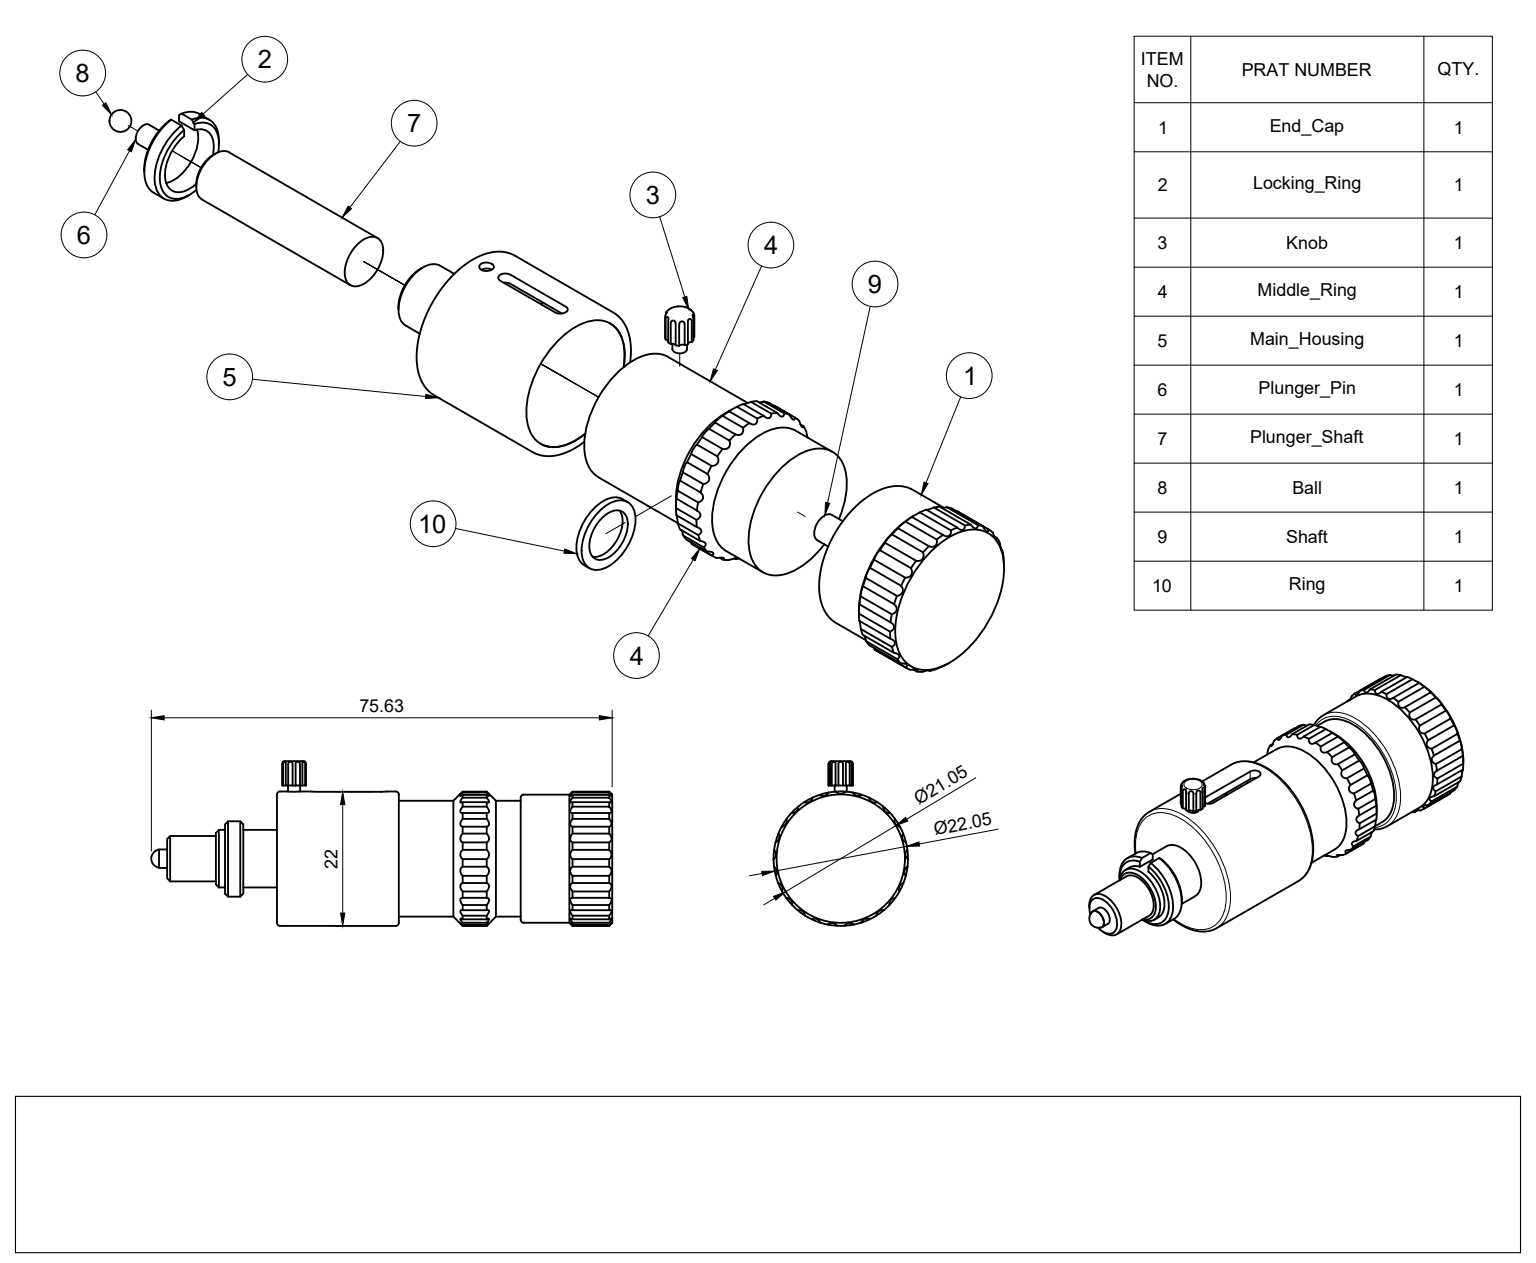
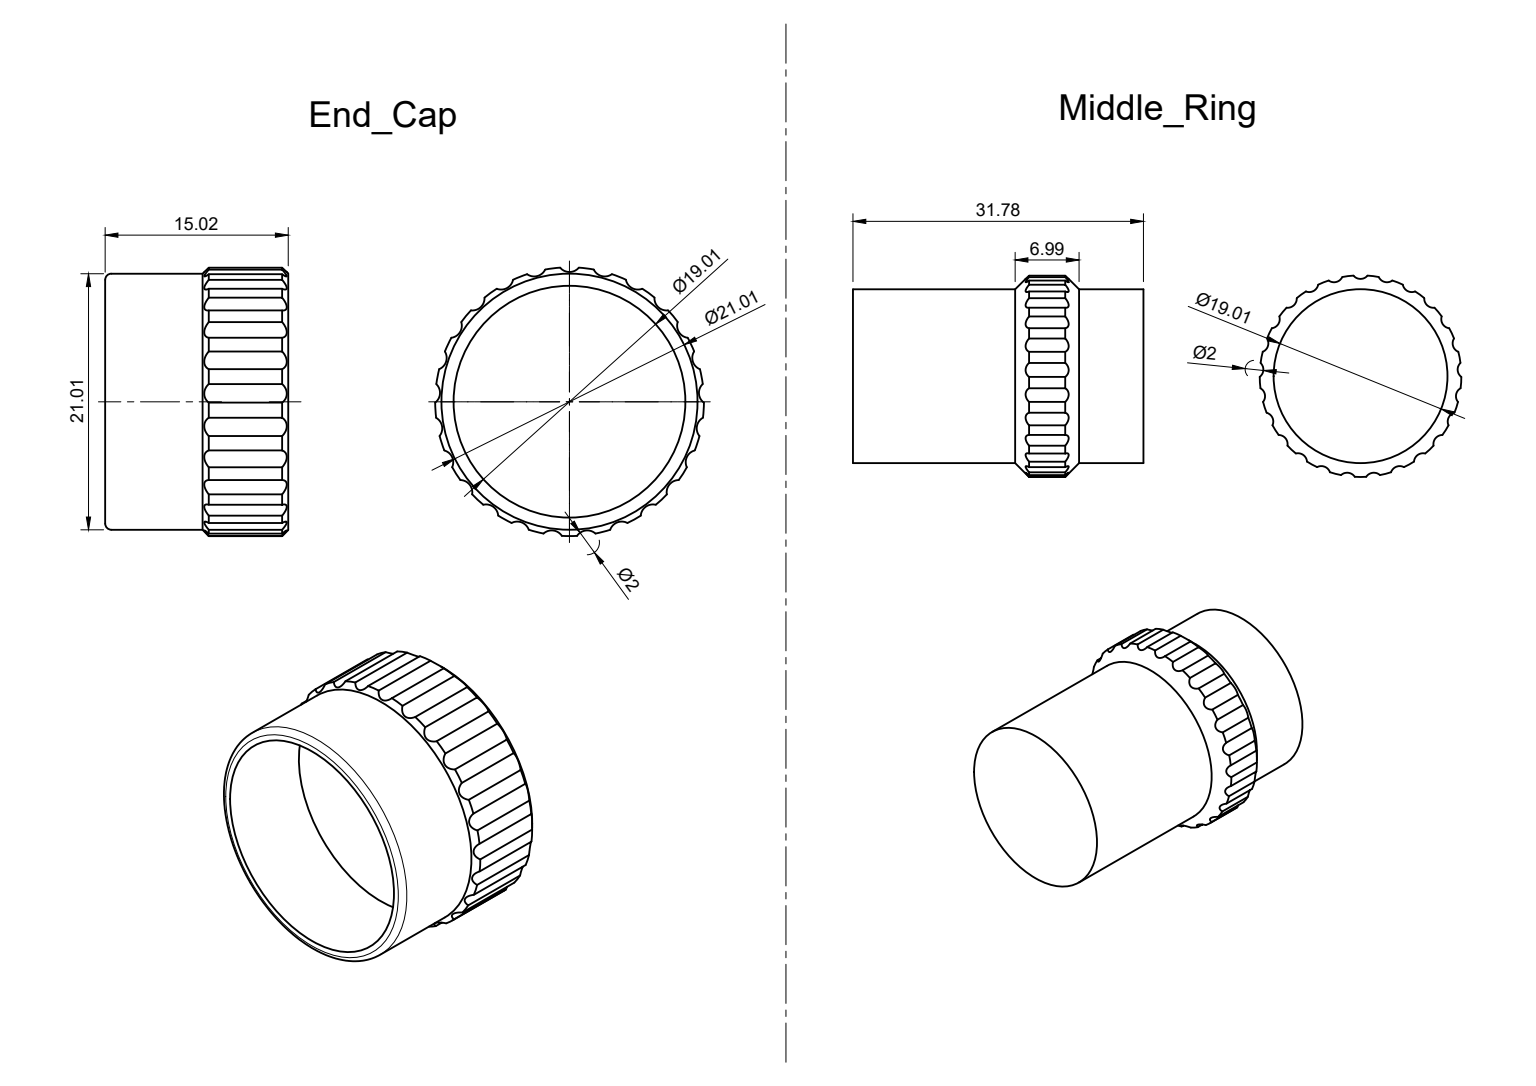
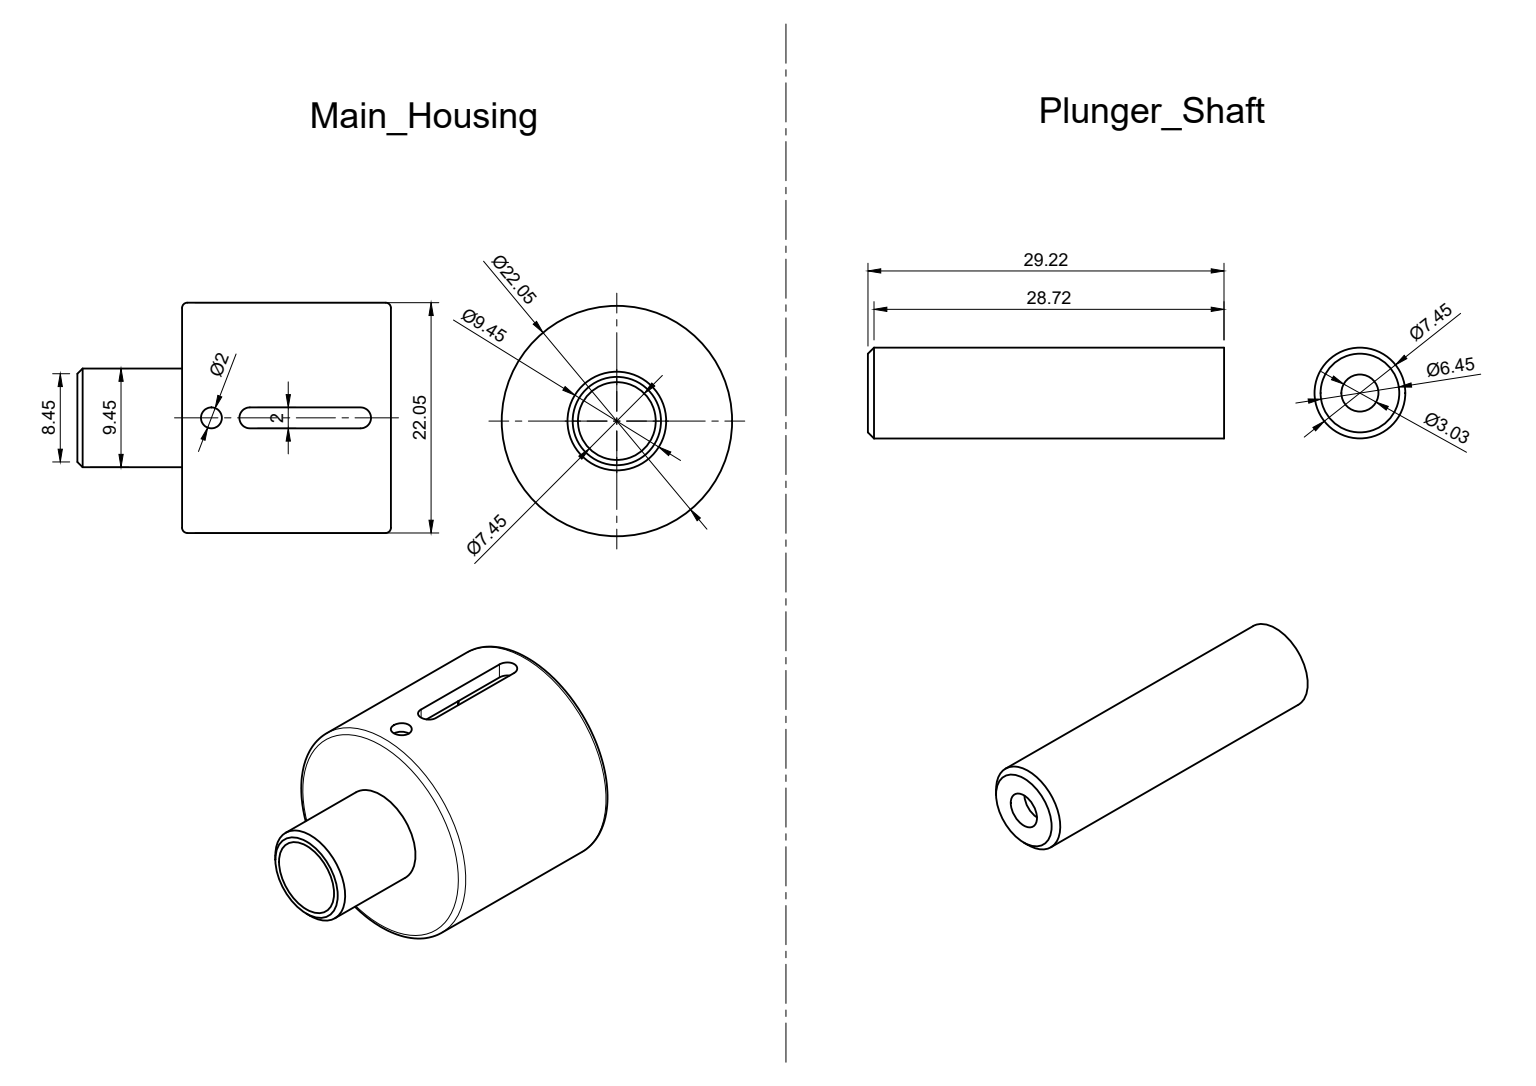
ISO-10303-21;
HEADER;
/* Generated by software containing ST-Developer
 * from STEP Tools, Inc. (www.steptools.com) 
 */

FILE_DESCRIPTION(
/* description */ (''),
/* implementation_level */ '2;1');

FILE_NAME(
/* name */ 'MAS-283',
/* time_stamp */ '2026-10-23T17:22:31+06:00',
/* author */ (''),
/* organization */ (''),
/* preprocessor_version */ 'ST-DEVELOPER v20.2',
/* originating_system */ 'Autodesk Translation Framework v15.15.0.0',
/* authorisation */ '');

FILE_SCHEMA (('AUTOMOTIVE_DESIGN { 1 0 10303 214 3 1 1 }'));
ENDSEC;

DATA;
#10=MECHANICAL_DESIGN_GEOMETRIC_PRESENTATION_REPRESENTATION('',(#77,#78,
#79,#80,#81,#82,#83,#84,#85,#86),#7315);
#11=ITEM_DEFINED_TRANSFORMATION($,$,#3336,#3714);
#12=ITEM_DEFINED_TRANSFORMATION($,$,#3452,#3715);
#13=ITEM_DEFINED_TRANSFORMATION($,$,#3467,#3716);
#14=ITEM_DEFINED_TRANSFORMATION($,$,#3527,#3717);
#15=ITEM_DEFINED_TRANSFORMATION($,$,#3638,#3718);
#16=ITEM_DEFINED_TRANSFORMATION($,$,#3673,#3719);
#17=ITEM_DEFINED_TRANSFORMATION($,$,#3684,#3720);
#18=ITEM_DEFINED_TRANSFORMATION($,$,#3696,#3721);
#19=ITEM_DEFINED_TRANSFORMATION($,$,#3699,#3722);
#20=ITEM_DEFINED_TRANSFORMATION($,$,#3705,#3723);
#21=(
REPRESENTATION_RELATIONSHIP($,$,#7353,#7352)
REPRESENTATION_RELATIONSHIP_WITH_TRANSFORMATION(#11)
SHAPE_REPRESENTATION_RELATIONSHIP()
);
#22=(
REPRESENTATION_RELATIONSHIP($,$,#7354,#7352)
REPRESENTATION_RELATIONSHIP_WITH_TRANSFORMATION(#12)
SHAPE_REPRESENTATION_RELATIONSHIP()
);
#23=(
REPRESENTATION_RELATIONSHIP($,$,#7355,#7352)
REPRESENTATION_RELATIONSHIP_WITH_TRANSFORMATION(#13)
SHAPE_REPRESENTATION_RELATIONSHIP()
);
#24=(
REPRESENTATION_RELATIONSHIP($,$,#7356,#7352)
REPRESENTATION_RELATIONSHIP_WITH_TRANSFORMATION(#14)
SHAPE_REPRESENTATION_RELATIONSHIP()
);
#25=(
REPRESENTATION_RELATIONSHIP($,$,#7357,#7352)
REPRESENTATION_RELATIONSHIP_WITH_TRANSFORMATION(#15)
SHAPE_REPRESENTATION_RELATIONSHIP()
);
#26=(
REPRESENTATION_RELATIONSHIP($,$,#7358,#7352)
REPRESENTATION_RELATIONSHIP_WITH_TRANSFORMATION(#16)
SHAPE_REPRESENTATION_RELATIONSHIP()
);
#27=(
REPRESENTATION_RELATIONSHIP($,$,#7359,#7352)
REPRESENTATION_RELATIONSHIP_WITH_TRANSFORMATION(#17)
SHAPE_REPRESENTATION_RELATIONSHIP()
);
#28=(
REPRESENTATION_RELATIONSHIP($,$,#7360,#7352)
REPRESENTATION_RELATIONSHIP_WITH_TRANSFORMATION(#18)
SHAPE_REPRESENTATION_RELATIONSHIP()
);
#29=(
REPRESENTATION_RELATIONSHIP($,$,#7361,#7352)
REPRESENTATION_RELATIONSHIP_WITH_TRANSFORMATION(#19)
SHAPE_REPRESENTATION_RELATIONSHIP()
);
#30=(
REPRESENTATION_RELATIONSHIP($,$,#7362,#7352)
REPRESENTATION_RELATIONSHIP_WITH_TRANSFORMATION(#20)
SHAPE_REPRESENTATION_RELATIONSHIP()
);
#31=CONTEXT_DEPENDENT_SHAPE_REPRESENTATION(#21,#7342);
#32=CONTEXT_DEPENDENT_SHAPE_REPRESENTATION(#22,#7343);
#33=CONTEXT_DEPENDENT_SHAPE_REPRESENTATION(#23,#7344);
#34=CONTEXT_DEPENDENT_SHAPE_REPRESENTATION(#24,#7345);
#35=CONTEXT_DEPENDENT_SHAPE_REPRESENTATION(#25,#7346);
#36=CONTEXT_DEPENDENT_SHAPE_REPRESENTATION(#26,#7347);
#37=CONTEXT_DEPENDENT_SHAPE_REPRESENTATION(#27,#7348);
#38=CONTEXT_DEPENDENT_SHAPE_REPRESENTATION(#28,#7349);
#39=CONTEXT_DEPENDENT_SHAPE_REPRESENTATION(#29,#7350);
#40=CONTEXT_DEPENDENT_SHAPE_REPRESENTATION(#30,#7351);
#41=NEXT_ASSEMBLY_USAGE_OCCURRENCE('End_Cap:1','End_Cap:1','End_Cap:1',
#7364,#7365,'End_Cap:1');
#42=NEXT_ASSEMBLY_USAGE_OCCURRENCE('Locking_Ring:1','Locking_Ring:1',
'Locking_Ring:1',#7364,#7366,'Locking_Ring:1');
#43=NEXT_ASSEMBLY_USAGE_OCCURRENCE('Knob:1','Knob:1','Knob:1',#7364,#7367,
'Knob:1');
#44=NEXT_ASSEMBLY_USAGE_OCCURRENCE('Middle_Ring:1','Middle_Ring:1',
'Middle_Ring:1',#7364,#7368,'Middle_Ring:1');
#45=NEXT_ASSEMBLY_USAGE_OCCURRENCE('Main_Housing:1','Main_Housing:1',
'Main_Housing:1',#7364,#7369,'Main_Housing:1');
#46=NEXT_ASSEMBLY_USAGE_OCCURRENCE('Plunger_Pin:1','Plunger_Pin:1',
'Plunger_Pin:1',#7364,#7370,'Plunger_Pin:1');
#47=NEXT_ASSEMBLY_USAGE_OCCURRENCE('Plunger_Shaft:1','Plunger_Shaft:1',
'Plunger_Shaft:1',#7364,#7371,'Plunger_Shaft:1');
#48=NEXT_ASSEMBLY_USAGE_OCCURRENCE('Ball:1','Ball:1','Ball:1',#7364,#7372,
'Ball:1');
#49=NEXT_ASSEMBLY_USAGE_OCCURRENCE('Shaft:1','Shaft:1','Shaft:1',#7364,
#7373,'Shaft:1');
#50=NEXT_ASSEMBLY_USAGE_OCCURRENCE('Ring:1','Ring:1','Ring:1',#7364,#7374,
'Ring:1');
#51=SPHERICAL_SURFACE('',#3674,1.5);
#52=SPHERICAL_SURFACE('',#3697,1.5);
#53=(
BOUNDED_CURVE()
B_SPLINE_CURVE(2,(#5649,#5650,#5651),.UNSPECIFIED.,.F.,.F.)
B_SPLINE_CURVE_WITH_KNOTS((3,3),(0.34166803276061,0.426429000654806),
 .UNSPECIFIED.)
CURVE()
GEOMETRIC_REPRESENTATION_ITEM()
RATIONAL_B_SPLINE_CURVE((1.00724935954325,1.0045238899297,1.))
REPRESENTATION_ITEM('')
);
#54=(
BOUNDED_CURVE()
B_SPLINE_CURVE(2,(#5655,#5656,#5657),.UNSPECIFIED.,.F.,.F.)
B_SPLINE_CURVE_WITH_KNOTS((3,3),(0.,0.0847609678918292),.UNSPECIFIED.)
CURVE()
GEOMETRIC_REPRESENTATION_ITEM()
RATIONAL_B_SPLINE_CURVE((1.,1.00452388992958,1.0072493595431))
REPRESENTATION_ITEM('')
);
#55=(
BOUNDED_CURVE()
B_SPLINE_CURVE(2,(#5669,#5670,#5671),.UNSPECIFIED.,.F.,.F.)
B_SPLINE_CURVE_WITH_KNOTS((3,3),(0.,0.0847609678918293),.UNSPECIFIED.)
CURVE()
GEOMETRIC_REPRESENTATION_ITEM()
RATIONAL_B_SPLINE_CURVE((1.,1.00452388992958,1.0072493595431))
REPRESENTATION_ITEM('')
);
#56=(
BOUNDED_CURVE()
B_SPLINE_CURVE(2,(#5678,#5679,#5680),.UNSPECIFIED.,.F.,.F.)
B_SPLINE_CURVE_WITH_KNOTS((3,3),(0.34166803276061,0.426429000654806),
 .UNSPECIFIED.)
CURVE()
GEOMETRIC_REPRESENTATION_ITEM()
RATIONAL_B_SPLINE_CURVE((1.00724935954325,1.0045238899297,1.))
REPRESENTATION_ITEM('')
);
#57=SHAPE_REPRESENTATION_RELATIONSHIP('SRR','None',#7353,#67);
#58=SHAPE_REPRESENTATION_RELATIONSHIP('SRR','None',#7354,#68);
#59=SHAPE_REPRESENTATION_RELATIONSHIP('SRR','None',#7355,#69);
#60=SHAPE_REPRESENTATION_RELATIONSHIP('SRR','None',#7356,#70);
#61=SHAPE_REPRESENTATION_RELATIONSHIP('SRR','None',#7357,#71);
#62=SHAPE_REPRESENTATION_RELATIONSHIP('SRR','None',#7358,#72);
#63=SHAPE_REPRESENTATION_RELATIONSHIP('SRR','None',#7359,#73);
#64=SHAPE_REPRESENTATION_RELATIONSHIP('SRR','None',#7360,#74);
#65=SHAPE_REPRESENTATION_RELATIONSHIP('SRR','None',#7361,#75);
#66=SHAPE_REPRESENTATION_RELATIONSHIP('SRR','None',#7362,#76);
#67=ADVANCED_BREP_SHAPE_REPRESENTATION('',(#87),#7305);
#68=ADVANCED_BREP_SHAPE_REPRESENTATION('',(#88),#7306);
#69=ADVANCED_BREP_SHAPE_REPRESENTATION('',(#89),#7307);
#70=ADVANCED_BREP_SHAPE_REPRESENTATION('',(#90),#7308);
#71=ADVANCED_BREP_SHAPE_REPRESENTATION('',(#91),#7309);
#72=ADVANCED_BREP_SHAPE_REPRESENTATION('',(#92),#7310);
#73=ADVANCED_BREP_SHAPE_REPRESENTATION('',(#93),#7311);
#74=ADVANCED_BREP_SHAPE_REPRESENTATION('',(#94),#7312);
#75=ADVANCED_BREP_SHAPE_REPRESENTATION('',(#95),#7313);
#76=ADVANCED_BREP_SHAPE_REPRESENTATION('',(#96),#7314);
#77=STYLED_ITEM('',(#7459),#87);
#78=STYLED_ITEM('',(#7438),#88);
#79=STYLED_ITEM('',(#7438),#89);
#80=STYLED_ITEM('',(#7431),#90);
#81=STYLED_ITEM('',(#7424),#91);
#82=STYLED_ITEM('',(#7445),#92);
#83=STYLED_ITEM('',(#7445),#93);
#84=STYLED_ITEM('',(#7431),#94);
#85=STYLED_ITEM('',(#7445),#95);
#86=STYLED_ITEM('',(#7431),#96);
#87=MANIFOLD_SOLID_BREP('End_Cap',#3214);
#88=MANIFOLD_SOLID_BREP('Locking_Ring',#3215);
#89=MANIFOLD_SOLID_BREP('Knob',#3216);
#90=MANIFOLD_SOLID_BREP('Middle_Ring',#3217);
#91=MANIFOLD_SOLID_BREP('Main_Housing',#3218);
#92=MANIFOLD_SOLID_BREP('Plunger_Pin',#3219);
#93=MANIFOLD_SOLID_BREP('Plunger_Shaft',#3220);
#94=MANIFOLD_SOLID_BREP('Ball',#3221);
#95=MANIFOLD_SOLID_BREP('Shaft',#3222);
#96=MANIFOLD_SOLID_BREP('Ring',#3223);
#97=CONICAL_SURFACE('',#3369,10.7746348408465,0.785398163397451);
#98=CONICAL_SURFACE('',#3445,10.765215394118,0.792062411554777);
#99=CONICAL_SURFACE('',#3453,5.97286361298787,0.785398163397449);
#100=CONICAL_SURFACE('',#3459,5.97286361298787,0.785398163397449);
#101=CONICAL_SURFACE('',#3552,10.265215394118,0.787617500807741);
#102=CONICAL_SURFACE('',#3635,10.265215394118,0.783178825987157);
#103=CONICAL_SURFACE('',#3651,4.47286361298787,0.785398163397448);
#104=CONICAL_SURFACE('',#3685,3.47286361298787,0.785398163397448);
#105=B_SPLINE_CURVE_WITH_KNOTS('',3,(#4680,#4681,#4682,#4683,#4684,#4685,
#4686,#4687,#4688,#4689,#4690,#4691,#4692,#4693),.UNSPECIFIED.,.F.,.F.,
(4,2,2,2,2,2,4),(0.0797634135970256,0.102765114722899,0.137781856198111,
0.172798597673324,0.207815339148536,0.242832080623748,0.265833781749622),
 .UNSPECIFIED.);
#106=B_SPLINE_CURVE_WITH_KNOTS('',3,(#4697,#4698,#4699,#4700,#4701,#4702,
#4703,#4704,#4705,#4706,#4707,#4708,#4709,#4710),.UNSPECIFIED.,.F.,.F.,
(4,2,2,2,2,2,4),(0.466800477660132,0.490054785503752,0.525068426419775,
0.560082067335798,0.595095708251821,0.630109349167844,0.653363657011464),
 .UNSPECIFIED.);
#107=B_SPLINE_CURVE_WITH_KNOTS('',3,(#4715,#4716,#4717,#4718,#4719,#4720,
#4721,#4722,#4723,#4724,#4725,#4726,#4727,#4728),.UNSPECIFIED.,.F.,.F.,
(4,2,2,2,2,2,4),(0.0797634135970254,0.102765114722899,0.137781856198111,
0.172798597673323,0.207815339148535,0.242832080623747,0.265833781749621),
 .UNSPECIFIED.);
#108=B_SPLINE_CURVE_WITH_KNOTS('',3,(#4732,#4733,#4734,#4735,#4736,#4737,
#4738,#4739,#4740,#4741,#4742,#4743,#4744,#4745),.UNSPECIFIED.,.F.,.F.,
(4,2,2,2,2,2,4),(0.466800477660133,0.490054785503752,0.525068426419776,
0.560082067335799,0.595095708251822,0.630109349167845,0.653363657011464),
 .UNSPECIFIED.);
#109=B_SPLINE_CURVE_WITH_KNOTS('',3,(#4750,#4751,#4752,#4753,#4754,#4755,
#4756,#4757,#4758,#4759,#4760,#4761,#4762,#4763),.UNSPECIFIED.,.F.,.F.,
(4,2,2,2,2,2,4),(0.0797634135970257,0.102765114722899,0.137781856198111,
0.172798597673324,0.207815339148536,0.242832080623748,0.265833781749623),
 .UNSPECIFIED.);
#110=B_SPLINE_CURVE_WITH_KNOTS('',3,(#4767,#4768,#4769,#4770,#4771,#4772,
#4773,#4774,#4775,#4776,#4777,#4778,#4779,#4780),.UNSPECIFIED.,.F.,.F.,
(4,2,2,2,2,2,4),(0.466800477660132,0.490054785503751,0.525068426419774,
0.560082067335798,0.595095708251821,0.630109349167844,0.653363657011463),
 .UNSPECIFIED.);
#111=B_SPLINE_CURVE_WITH_KNOTS('',3,(#4785,#4786,#4787,#4788,#4789,#4790,
#4791,#4792,#4793,#4794,#4795,#4796,#4797,#4798),.UNSPECIFIED.,.F.,.F.,
(4,2,2,2,2,2,4),(0.0797634135970255,0.102765114722899,0.137781856198111,
0.172798597673323,0.207815339148536,0.242832080623748,0.265833781749622),
 .UNSPECIFIED.);
#112=B_SPLINE_CURVE_WITH_KNOTS('',3,(#4802,#4803,#4804,#4805,#4806,#4807,
#4808,#4809,#4810,#4811,#4812,#4813,#4814,#4815),.UNSPECIFIED.,.F.,.F.,
(4,2,2,2,2,2,4),(0.466800477660132,0.490054785503752,0.525068426419775,
0.560082067335798,0.595095708251821,0.630109349167844,0.653363657011464),
 .UNSPECIFIED.);
#113=B_SPLINE_CURVE_WITH_KNOTS('',3,(#4820,#4821,#4822,#4823,#4824,#4825,
#4826,#4827,#4828,#4829,#4830,#4831,#4832,#4833),.UNSPECIFIED.,.F.,.F.,
(4,2,2,2,2,2,4),(0.0797634135970245,0.102765114722899,0.137781856198111,
0.172798597673324,0.207815339148536,0.242832080623748,0.265833781749621),
 .UNSPECIFIED.);
#114=B_SPLINE_CURVE_WITH_KNOTS('',3,(#4837,#4838,#4839,#4840,#4841,#4842,
#4843,#4844,#4845,#4846,#4847,#4848,#4849,#4850),.UNSPECIFIED.,.F.,.F.,
(4,2,2,2,2,2,4),(0.466800477660132,0.490054785503751,0.525068426419774,
0.560082067335797,0.59509570825182,0.630109349167844,0.653363657011463),
 .UNSPECIFIED.);
#115=B_SPLINE_CURVE_WITH_KNOTS('',3,(#4855,#4856,#4857,#4858,#4859,#4860,
#4861,#4862,#4863,#4864,#4865,#4866,#4867,#4868),.UNSPECIFIED.,.F.,.F.,
(4,2,2,2,2,2,4),(0.0797634135970255,0.102765114722899,0.137781856198111,
0.172798597673324,0.207815339148536,0.242832080623748,0.265833781749622),
 .UNSPECIFIED.);
#116=B_SPLINE_CURVE_WITH_KNOTS('',3,(#4872,#4873,#4874,#4875,#4876,#4877,
#4878,#4879,#4880,#4881,#4882,#4883,#4884,#4885),.UNSPECIFIED.,.F.,.F.,
(4,2,2,2,2,2,4),(0.466800477660132,0.490054785503752,0.525068426419775,
0.560082067335798,0.595095708251821,0.630109349167844,0.653363657011464),
 .UNSPECIFIED.);
#117=B_SPLINE_CURVE_WITH_KNOTS('',3,(#4890,#4891,#4892,#4893,#4894,#4895,
#4896,#4897,#4898,#4899,#4900,#4901,#4902,#4903),.UNSPECIFIED.,.F.,.F.,
(4,2,2,2,2,2,4),(0.0797634135970254,0.102765114722899,0.137781856198111,
0.172798597673323,0.207815339148536,0.242832080623748,0.265833781749621),
 .UNSPECIFIED.);
#118=B_SPLINE_CURVE_WITH_KNOTS('',3,(#4907,#4908,#4909,#4910,#4911,#4912,
#4913,#4914,#4915,#4916,#4917,#4918,#4919,#4920),.UNSPECIFIED.,.F.,.F.,
(4,2,2,2,2,2,4),(0.466800477660132,0.490054785503752,0.525068426419775,
0.560082067335798,0.595095708251821,0.630109349167844,0.653363657011464),
 .UNSPECIFIED.);
#119=B_SPLINE_CURVE_WITH_KNOTS('',3,(#4925,#4926,#4927,#4928,#4929,#4930,
#4931,#4932,#4933,#4934,#4935,#4936,#4937,#4938),.UNSPECIFIED.,.F.,.F.,
(4,2,2,2,2,2,4),(0.0797634135970265,0.1027651147229,0.137781856198112,0.172798597673324,
0.207815339148536,0.242832080623748,0.265833781749622),.UNSPECIFIED.);
#120=B_SPLINE_CURVE_WITH_KNOTS('',3,(#4942,#4943,#4944,#4945,#4946,#4947,
#4948,#4949,#4950,#4951,#4952,#4953,#4954,#4955),.UNSPECIFIED.,.F.,.F.,
(4,2,2,2,2,2,4),(0.466800477660132,0.490054785503752,0.525068426419775,
0.560082067335798,0.595095708251821,0.630109349167844,0.653363657011464),
 .UNSPECIFIED.);
#121=B_SPLINE_CURVE_WITH_KNOTS('',3,(#4960,#4961,#4962,#4963,#4964,#4965,
#4966,#4967,#4968,#4969,#4970,#4971,#4972,#4973),.UNSPECIFIED.,.F.,.F.,
(4,2,2,2,2,2,4),(0.0797634135970254,0.102765114722899,0.137781856198111,
0.172798597673323,0.207815339148535,0.242832080623747,0.265833781749621),
 .UNSPECIFIED.);
#122=B_SPLINE_CURVE_WITH_KNOTS('',3,(#4977,#4978,#4979,#4980,#4981,#4982,
#4983,#4984,#4985,#4986,#4987,#4988,#4989,#4990),.UNSPECIFIED.,.F.,.F.,
(4,2,2,2,2,2,4),(0.466800477660131,0.490054785503751,0.525068426419774,
0.560082067335798,0.59509570825182,0.630109349167843,0.653363657011463),
 .UNSPECIFIED.);
#123=B_SPLINE_CURVE_WITH_KNOTS('',3,(#4995,#4996,#4997,#4998,#4999,#5000,
#5001,#5002,#5003,#5004,#5005,#5006,#5007,#5008),.UNSPECIFIED.,.F.,.F.,
(4,2,2,2,2,2,4),(0.0797634135970272,0.102765114722899,0.137781856198112,
0.172798597673324,0.207815339148536,0.242832080623748,0.265833781749622),
 .UNSPECIFIED.);
#124=B_SPLINE_CURVE_WITH_KNOTS('',3,(#5012,#5013,#5014,#5015,#5016,#5017,
#5018,#5019,#5020,#5021,#5022,#5023,#5024,#5025),.UNSPECIFIED.,.F.,.F.,
(4,2,2,2,2,2,4),(0.466800477660132,0.490054785503752,0.525068426419775,
0.560082067335798,0.595095708251821,0.630109349167844,0.653363657011464),
 .UNSPECIFIED.);
#125=B_SPLINE_CURVE_WITH_KNOTS('',3,(#5030,#5031,#5032,#5033,#5034,#5035,
#5036,#5037,#5038,#5039,#5040,#5041,#5042,#5043),.UNSPECIFIED.,.F.,.F.,
(4,2,2,2,2,2,4),(0.0797634135970255,0.102765114722899,0.137781856198111,
0.172798597673323,0.207815339148535,0.242832080623748,0.265833781749622),
 .UNSPECIFIED.);
#126=B_SPLINE_CURVE_WITH_KNOTS('',3,(#5047,#5048,#5049,#5050,#5051,#5052,
#5053,#5054,#5055,#5056,#5057,#5058,#5059,#5060),.UNSPECIFIED.,.F.,.F.,
(4,2,2,2,2,2,4),(0.466800477660132,0.490054785503752,0.525068426419775,
0.560082067335798,0.595095708251821,0.630109349167844,0.653363657011464),
 .UNSPECIFIED.);
#127=B_SPLINE_CURVE_WITH_KNOTS('',3,(#5065,#5066,#5067,#5068,#5069,#5070,
#5071,#5072,#5073,#5074,#5075,#5076,#5077,#5078),.UNSPECIFIED.,.F.,.F.,
(4,2,2,2,2,2,4),(0.0797634135970258,0.102765114722899,0.137781856198111,
0.172798597673324,0.207815339148536,0.242832080623748,0.265833781749623),
 .UNSPECIFIED.);
#128=B_SPLINE_CURVE_WITH_KNOTS('',3,(#5082,#5083,#5084,#5085,#5086,#5087,
#5088,#5089,#5090,#5091,#5092,#5093,#5094,#5095),.UNSPECIFIED.,.F.,.F.,
(4,2,2,2,2,2,4),(0.466800477660132,0.490054785503751,0.525068426419774,
0.560082067335797,0.59509570825182,0.630109349167844,0.653363657011463),
 .UNSPECIFIED.);
#129=B_SPLINE_CURVE_WITH_KNOTS('',3,(#5100,#5101,#5102,#5103,#5104,#5105,
#5106,#5107,#5108,#5109,#5110,#5111,#5112,#5113),.UNSPECIFIED.,.F.,.F.,
(4,2,2,2,2,2,4),(0.0797634135970256,0.102765114722899,0.137781856198111,
0.172798597673324,0.207815339148536,0.242832080623748,0.265833781749621),
 .UNSPECIFIED.);
#130=B_SPLINE_CURVE_WITH_KNOTS('',3,(#5117,#5118,#5119,#5120,#5121,#5122,
#5123,#5124,#5125,#5126,#5127,#5128,#5129,#5130),.UNSPECIFIED.,.F.,.F.,
(4,2,2,2,2,2,4),(0.466800477660132,0.490054785503751,0.525068426419774,
0.560082067335797,0.595095708251821,0.630109349167844,0.653363657011463),
 .UNSPECIFIED.);
#131=B_SPLINE_CURVE_WITH_KNOTS('',3,(#5135,#5136,#5137,#5138,#5139,#5140,
#5141,#5142,#5143,#5144,#5145,#5146,#5147,#5148),.UNSPECIFIED.,.F.,.F.,
(4,2,2,2,2,2,4),(0.0797634135970255,0.102765114722899,0.137781856198111,
0.172798597673323,0.207815339148536,0.242832080623748,0.265833781749622),
 .UNSPECIFIED.);
#132=B_SPLINE_CURVE_WITH_KNOTS('',3,(#5152,#5153,#5154,#5155,#5156,#5157,
#5158,#5159,#5160,#5161,#5162,#5163,#5164,#5165),.UNSPECIFIED.,.F.,.F.,
(4,2,2,2,2,2,4),(0.466800477660132,0.490054785503751,0.525068426419775,
0.560082067335798,0.595095708251821,0.630109349167844,0.653363657011464),
 .UNSPECIFIED.);
#133=B_SPLINE_CURVE_WITH_KNOTS('',3,(#5170,#5171,#5172,#5173,#5174,#5175,
#5176,#5177,#5178,#5179,#5180,#5181,#5182,#5183),.UNSPECIFIED.,.F.,.F.,
(4,2,2,2,2,2,4),(0.0797634135970253,0.102765114722899,0.137781856198111,
0.172798597673323,0.207815339148536,0.242832080623748,0.265833781749621),
 .UNSPECIFIED.);
#134=B_SPLINE_CURVE_WITH_KNOTS('',3,(#5187,#5188,#5189,#5190,#5191,#5192,
#5193,#5194,#5195,#5196,#5197,#5198,#5199,#5200),.UNSPECIFIED.,.F.,.F.,
(4,2,2,2,2,2,4),(0.466800477660132,0.490054785503751,0.525068426419775,
0.560082067335798,0.595095708251821,0.630109349167844,0.653363657011464),
 .UNSPECIFIED.);
#135=B_SPLINE_CURVE_WITH_KNOTS('',3,(#5205,#5206,#5207,#5208,#5209,#5210,
#5211,#5212,#5213,#5214,#5215,#5216,#5217,#5218),.UNSPECIFIED.,.F.,.F.,
(4,2,2,2,2,2,4),(0.0797634135970255,0.102765114722899,0.137781856198111,
0.172798597673323,0.207815339148536,0.242832080623748,0.265833781749622),
 .UNSPECIFIED.);
#136=B_SPLINE_CURVE_WITH_KNOTS('',3,(#5222,#5223,#5224,#5225,#5226,#5227,
#5228,#5229,#5230,#5231,#5232,#5233,#5234,#5235),.UNSPECIFIED.,.F.,.F.,
(4,2,2,2,2,2,4),(0.466800477660132,0.490054785503751,0.525068426419775,
0.560082067335798,0.595095708251821,0.630109349167844,0.653363657011463),
 .UNSPECIFIED.);
#137=B_SPLINE_CURVE_WITH_KNOTS('',3,(#5240,#5241,#5242,#5243,#5244,#5245,
#5246,#5247,#5248,#5249,#5250,#5251,#5252,#5253),.UNSPECIFIED.,.F.,.F.,
(4,2,2,2,2,2,4),(0.0797634135970254,0.102765114722899,0.137781856198111,
0.172798597673323,0.207815339148535,0.242832080623747,0.265833781749621),
 .UNSPECIFIED.);
#138=B_SPLINE_CURVE_WITH_KNOTS('',3,(#5257,#5258,#5259,#5260,#5261,#5262,
#5263,#5264,#5265,#5266,#5267,#5268,#5269,#5270),.UNSPECIFIED.,.F.,.F.,
(4,2,2,2,2,2,4),(0.466800477660132,0.490054785503752,0.525068426419775,
0.560082067335798,0.595095708251821,0.630109349167844,0.653363657011464),
 .UNSPECIFIED.);
#139=B_SPLINE_CURVE_WITH_KNOTS('',3,(#5275,#5276,#5277,#5278,#5279,#5280,
#5281,#5282,#5283,#5284,#5285,#5286,#5287,#5288),.UNSPECIFIED.,.F.,.F.,
(4,2,2,2,2,2,4),(0.0797634135970276,0.102765114722899,0.137781856198111,
0.172798597673324,0.207815339148536,0.242832080623748,0.265833781749621),
 .UNSPECIFIED.);
#140=B_SPLINE_CURVE_WITH_KNOTS('',3,(#5292,#5293,#5294,#5295,#5296,#5297,
#5298,#5299,#5300,#5301,#5302,#5303,#5304,#5305),.UNSPECIFIED.,.F.,.F.,
(4,2,2,2,2,2,4),(0.466800477660133,0.490054785503752,0.525068426419776,
0.560082067335799,0.595095708251822,0.630109349167845,0.653363657011464),
 .UNSPECIFIED.);
#141=B_SPLINE_CURVE_WITH_KNOTS('',3,(#5310,#5311,#5312,#5313,#5314,#5315,
#5316,#5317,#5318,#5319,#5320,#5321,#5322,#5323),.UNSPECIFIED.,.F.,.F.,
(4,2,2,2,2,2,4),(0.0797634135970256,0.102765114722899,0.137781856198112,
0.172798597673324,0.207815339148536,0.242832080623748,0.265833781749622),
 .UNSPECIFIED.);
#142=B_SPLINE_CURVE_WITH_KNOTS('',3,(#5327,#5328,#5329,#5330,#5331,#5332,
#5333,#5334,#5335,#5336,#5337,#5338,#5339,#5340),.UNSPECIFIED.,.F.,.F.,
(4,2,2,2,2,2,4),(0.466800477660132,0.490054785503752,0.525068426419775,
0.560082067335798,0.595095708251822,0.630109349167845,0.653363657011465),
 .UNSPECIFIED.);
#143=B_SPLINE_CURVE_WITH_KNOTS('',3,(#5345,#5346,#5347,#5348,#5349,#5350,
#5351,#5352,#5353,#5354,#5355,#5356,#5357,#5358),.UNSPECIFIED.,.F.,.F.,
(4,2,2,2,2,2,4),(0.0797634135970255,0.102765114722899,0.137781856198111,
0.172798597673323,0.207815339148536,0.242832080623748,0.265833781749621),
 .UNSPECIFIED.);
#144=B_SPLINE_CURVE_WITH_KNOTS('',3,(#5362,#5363,#5364,#5365,#5366,#5367,
#5368,#5369,#5370,#5371,#5372,#5373,#5374,#5375),.UNSPECIFIED.,.F.,.F.,
(4,2,2,2,2,2,4),(0.466800477660133,0.490054785503752,0.525068426419775,
0.560082067335798,0.595095708251821,0.630109349167844,0.653363657011464),
 .UNSPECIFIED.);
#145=B_SPLINE_CURVE_WITH_KNOTS('',3,(#5380,#5381,#5382,#5383,#5384,#5385,
#5386,#5387,#5388,#5389,#5390,#5391,#5392,#5393),.UNSPECIFIED.,.F.,.F.,
(4,2,2,2,2,2,4),(0.0797634135970255,0.102765114722899,0.137781856198111,
0.172798597673323,0.207815339148536,0.242832080623748,0.265833781749621),
 .UNSPECIFIED.);
#146=B_SPLINE_CURVE_WITH_KNOTS('',3,(#5397,#5398,#5399,#5400,#5401,#5402,
#5403,#5404,#5405,#5406,#5407,#5408,#5409,#5410),.UNSPECIFIED.,.F.,.F.,
(4,2,2,2,2,2,4),(0.466800477660132,0.490054785503752,0.525068426419775,
0.560082067335798,0.595095708251821,0.630109349167844,0.653363657011464),
 .UNSPECIFIED.);
#147=B_SPLINE_CURVE_WITH_KNOTS('',3,(#5415,#5416,#5417,#5418,#5419,#5420,
#5421,#5422,#5423,#5424,#5425,#5426,#5427,#5428),.UNSPECIFIED.,.F.,.F.,
(4,2,2,2,2,2,4),(0.0797634135970255,0.102765114722899,0.137781856198111,
0.172798597673324,0.207815339148536,0.242832080623748,0.265833781749623),
 .UNSPECIFIED.);
#148=B_SPLINE_CURVE_WITH_KNOTS('',3,(#5432,#5433,#5434,#5435,#5436,#5437,
#5438,#5439,#5440,#5441,#5442,#5443,#5444,#5445),.UNSPECIFIED.,.F.,.F.,
(4,2,2,2,2,2,4),(0.466800477660132,0.490054785503752,0.525068426419775,
0.560082067335798,0.595095708251821,0.630109349167844,0.653363657011463),
 .UNSPECIFIED.);
#149=B_SPLINE_CURVE_WITH_KNOTS('',3,(#5450,#5451,#5452,#5453,#5454,#5455,
#5456,#5457,#5458,#5459,#5460,#5461,#5462,#5463),.UNSPECIFIED.,.F.,.F.,
(4,2,2,2,2,2,4),(0.0797634135970256,0.102765114722899,0.137781856198111,
0.172798597673323,0.207815339148536,0.242832080623748,0.265833781749621),
 .UNSPECIFIED.);
#150=B_SPLINE_CURVE_WITH_KNOTS('',3,(#5467,#5468,#5469,#5470,#5471,#5472,
#5473,#5474,#5475,#5476,#5477,#5478,#5479,#5480),.UNSPECIFIED.,.F.,.F.,
(4,2,2,2,2,2,4),(0.466800477660132,0.490054785503752,0.525068426419775,
0.560082067335798,0.595095708251821,0.630109349167844,0.653363657011463),
 .UNSPECIFIED.);
#151=B_SPLINE_CURVE_WITH_KNOTS('',3,(#5485,#5486,#5487,#5488,#5489,#5490,
#5491,#5492,#5493,#5494,#5495,#5496,#5497,#5498),.UNSPECIFIED.,.F.,.F.,
(4,2,2,2,2,2,4),(0.0797634135970257,0.102765114722899,0.137781856198111,
0.172798597673324,0.207815339148536,0.242832080623748,0.265833781749622),
 .UNSPECIFIED.);
#152=B_SPLINE_CURVE_WITH_KNOTS('',3,(#5502,#5503,#5504,#5505,#5506,#5507,
#5508,#5509,#5510,#5511,#5512,#5513,#5514,#5515),.UNSPECIFIED.,.F.,.F.,
(4,2,2,2,2,2,4),(0.466800477660132,0.490054785503752,0.525068426419775,
0.560082067335798,0.595095708251821,0.630109349167844,0.653363657011463),
 .UNSPECIFIED.);
#153=B_SPLINE_CURVE_WITH_KNOTS('',3,(#5523,#5524,#5525,#5526,#5527,#5528,
#5529,#5530),.UNSPECIFIED.,.F.,.F.,(4,2,2,4),(0.560082067335798,0.595095708251821,
0.630109349167844,0.653363657011463),.UNSPECIFIED.);
#154=B_SPLINE_CURVE_WITH_KNOTS('',3,(#5557,#5558,#5559,#5560,#5561,#5562,
#5563,#5564),.UNSPECIFIED.,.F.,.F.,(4,2,2,4),(0.466800477660132,0.490054785503752,
0.525068426419775,0.560082067335798),.UNSPECIFIED.);
#155=B_SPLINE_CURVE_WITH_KNOTS('',3,(#5619,#5620,#5621,#5622,#5623,#5624,
#5625,#5626),.UNSPECIFIED.,.F.,.F.,(4,2,2,4),(0.0797634135970255,0.102765114722899,
0.137781856198111,0.172798597673323),.UNSPECIFIED.);
#156=B_SPLINE_CURVE_WITH_KNOTS('',3,(#5627,#5628,#5629,#5630,#5631,#5632,
#5633,#5634),.UNSPECIFIED.,.F.,.F.,(4,2,2,4),(0.172798597673323,0.207815339148535,
0.242832080623748,0.265833781749621),.UNSPECIFIED.);
#157=B_SPLINE_CURVE_WITH_KNOTS('',3,(#5698,#5699,#5700,#5701,#5702,#5703,
#5704,#5705,#5706,#5707,#5708,#5709,#5710,#5711,#5712,#5713,#5714,#5715,
#5716,#5717,#5718,#5719),.UNSPECIFIED.,.F.,.F.,(4,2,2,2,2,2,2,2,2,2,4),
(-0.134540802780941,-0.124694593380528,-0.114887429972743,-0.100865411229465,
-0.0874132288816555,-0.0739776319181918,-0.0597069979702496,-0.0456321639023999,
-0.0321262367963484,-0.0169842646851755,-7.43769472487735E-6),
 .UNSPECIFIED.);
#158=B_SPLINE_CURVE_WITH_KNOTS('',3,(#5728,#5729,#5730,#5731,#5732,#5733,
#5734,#5735,#5736,#5737,#5738,#5739,#5740,#5741,#5742,#5743,#5744,#5745,
#5746,#5747,#5748,#5749),.UNSPECIFIED.,.F.,.F.,(4,2,2,2,2,2,2,2,2,2,4),
(-0.134546412264088,-0.12503895955274,-0.115553020431079,-0.101555833168035,
-0.0880617151829101,-0.0742479340082139,-0.0594501685168066,-0.0457182707143297,
-0.0321286187319872,-0.0169925187729982,-7.43769474437564E-6),
 .UNSPECIFIED.);
#159=B_SPLINE_CURVE_WITH_KNOTS('',3,(#5758,#5759,#5760,#5761,#5762,#5763,
#5764,#5765,#5766,#5767,#5768,#5769,#5770,#5771,#5772,#5773,#5774,#5775,
#5776,#5777,#5778,#5779),.UNSPECIFIED.,.F.,.F.,(4,2,2,2,2,2,2,2,2,2,4),
(-0.134546412264079,-0.125038959552735,-0.115553020431074,-0.101555833168028,
-0.0880617151829049,-0.074247934008211,-0.0594501685168069,-0.0457182707143326,
-0.0321286187319901,-0.0169925187729991,-7.43769474460115E-6),
 .UNSPECIFIED.);
#160=B_SPLINE_CURVE_WITH_KNOTS('',3,(#5788,#5789,#5790,#5791,#5792,#5793,
#5794,#5795,#5796,#5797,#5798,#5799,#5800,#5801,#5802,#5803,#5804,#5805,
#5806,#5807,#5808,#5809),.UNSPECIFIED.,.F.,.F.,(4,2,2,2,2,2,2,2,2,2,4),
(-0.134540616537392,-0.124646722470156,-0.114789241819855,-0.100787758586552,
-0.0873465389988059,-0.0739206374616,-0.0596515865040428,-0.0456502398664556,
-0.0321268160753299,-0.0169860369506264,-7.43769472906497E-6),
 .UNSPECIFIED.);
#161=B_SPLINE_CURVE_WITH_KNOTS('',3,(#5818,#5819,#5820,#5821,#5822,#5823,
#5824,#5825,#5826,#5827,#5828,#5829,#5830,#5831,#5832,#5833,#5834,#5835,
#5836,#5837,#5838,#5839,#5840,#5841,#5842,#5843),.UNSPECIFIED.,.F.,.F.,
(4,2,2,2,2,2,2,2,2,2,2,2,4),(-0.134481588819224,-0.12541821251768,-0.116248820382152,
-0.10297112990022,-0.0890270299810203,-0.0783509942952859,-0.0707062224441527,
-0.0638270554385495,-0.0561931432260482,-0.0455507450931791,-0.031889734739909,
-0.0168775831944051,-7.43769447408144E-6),.UNSPECIFIED.);
#162=B_SPLINE_CURVE_WITH_KNOTS('',3,(#5852,#5853,#5854,#5855,#5856,#5857,
#5858,#5859,#5860,#5861,#5862,#5863,#5864,#5865,#5866,#5867,#5868,#5869,
#5870,#5871,#5872,#5873),.UNSPECIFIED.,.F.,.F.,(4,2,2,2,2,2,2,2,2,2,4),
(-0.134540616537393,-0.124646722470158,-0.114789241819856,-0.100787758586554,
-0.087346538998809,-0.0739206374616026,-0.0596515865040475,-0.0456502398664592,
-0.0321268160753317,-0.0169860369506279,-7.43769472906497E-6),
 .UNSPECIFIED.);
#163=B_SPLINE_CURVE_WITH_KNOTS('',3,(#5882,#5883,#5884,#5885,#5886,#5887,
#5888,#5889,#5890,#5891,#5892,#5893,#5894,#5895,#5896,#5897,#5898,#5899,
#5900,#5901,#5902,#5903),.UNSPECIFIED.,.F.,.F.,(4,2,2,2,2,2,2,2,2,2,4),
(-0.134546412264079,-0.125038959552731,-0.115553020431069,-0.101555833168023,
-0.0880617151828988,-0.0742479340082045,-0.0594501685167969,-0.0457182707143222,
-0.0321286187319822,-0.0169925187729959,-7.43769474437564E-6),
 .UNSPECIFIED.);
#164=B_SPLINE_CURVE_WITH_KNOTS('',3,(#5912,#5913,#5914,#5915,#5916,#5917,
#5918,#5919,#5920,#5921,#5922,#5923,#5924,#5925,#5926,#5927,#5928,#5929,
#5930,#5931,#5932,#5933),.UNSPECIFIED.,.F.,.F.,(4,2,2,2,2,2,2,2,2,2,4),
(-0.134546412264076,-0.125038959552731,-0.11555302043107,-0.101555833168024,
-0.0880617151829001,-0.0742479340082053,-0.0594501685167959,-0.0457182707143225,
-0.0321286187319831,-0.0169925187729947,-7.43769474415359E-6),
 .UNSPECIFIED.);
#165=B_SPLINE_CURVE_WITH_KNOTS('',3,(#5942,#5943,#5944,#5945,#5946,#5947,
#5948,#5949,#5950,#5951,#5952,#5953,#5954,#5955,#5956,#5957,#5958,#5959,
#5960,#5961,#5962,#5963),.UNSPECIFIED.,.F.,.F.,(4,2,2,2,2,2,2,2,2,2,4),
(-0.134540802780906,-0.124694593380492,-0.114887429972709,-0.100865411229438,
-0.0874132288816369,-0.0739776319181792,-0.0597069979702393,-0.0456321639023924,
-0.0321262367963445,-0.0169842646851756,-7.43769472488082E-6),
 .UNSPECIFIED.);
#166=B_SPLINE_CURVE_WITH_KNOTS('',3,(#6008,#6009,#6010,#6011,#6012,#6013,
#6014,#6015,#6016,#6017,#6018,#6019),.UNSPECIFIED.,.F.,.F.,(4,2,2,2,2,4),
(-0.0672537780264869,-0.0571863690452376,-0.0459002523768814,-0.0321135744364736,
-0.0170527660266752,0.),.UNSPECIFIED.);
#167=B_SPLINE_CURVE_WITH_KNOTS('',3,(#6022,#6023,#6024,#6025,#6026,#6027,
#6028,#6029,#6030,#6031,#6032,#6033,#6034,#6035,#6036,#6037),
 .UNSPECIFIED.,.F.,.F.,(4,2,2,2,2,2,2,4),(-0.134507884019342,-0.12584488585901,
-0.117135322530839,-0.103482612739793,-0.0895114384281185,-0.0780993566612536,
-0.0676309733624946,-0.0672537780264869),.UNSPECIFIED.);
#168=B_SPLINE_CURVE_WITH_KNOTS('',3,(#6051,#6052,#6053,#6054,#6055,#6056,
#6057,#6058,#6059,#6060,#6061,#6062,#6063,#6064),.UNSPECIFIED.,.F.,.F.,
(4,2,2,2,2,2,4),(0.0804140797636754,0.103753655307869,0.138766322922265,
0.173778990536662,0.208791658151058,0.243804325765454,0.267143901309648),
 .UNSPECIFIED.);
#169=B_SPLINE_CURVE_WITH_KNOTS('',3,(#6068,#6069,#6070,#6071,#6072,#6073,
#6074,#6075,#6076,#6077,#6078,#6079,#6080,#6081),.UNSPECIFIED.,.F.,.F.,
(4,2,2,2,2,2,4),(0.466102891398403,0.489272506433,0.524287150622646,0.559301794812291,
0.594316439001936,0.629331083191581,0.652500698226179),.UNSPECIFIED.);
#170=B_SPLINE_CURVE_WITH_KNOTS('',3,(#6086,#6087,#6088,#6089,#6090,#6091,
#6092,#6093,#6094,#6095,#6096,#6097,#6098,#6099),.UNSPECIFIED.,.F.,.F.,
(4,2,2,2,2,2,4),(0.0804140797636753,0.103753655307869,0.138766322922265,
0.173778990536662,0.208791658151058,0.243804325765454,0.267143901309648),
 .UNSPECIFIED.);
#171=B_SPLINE_CURVE_WITH_KNOTS('',3,(#6103,#6104,#6105,#6106,#6107,#6108,
#6109,#6110,#6111,#6112,#6113,#6114,#6115,#6116),.UNSPECIFIED.,.F.,.F.,
(4,2,2,2,2,2,4),(0.466102891398403,0.489272506433,0.524287150622645,0.55930179481229,
0.594316439001936,0.629331083191581,0.652500698226178),.UNSPECIFIED.);
#172=B_SPLINE_CURVE_WITH_KNOTS('',3,(#6121,#6122,#6123,#6124,#6125,#6126,
#6127,#6128,#6129,#6130,#6131,#6132,#6133,#6134),.UNSPECIFIED.,.F.,.F.,
(4,2,2,2,2,2,4),(0.0804140797636755,0.103753655307869,0.138766322922265,
0.173778990536661,0.208791658151058,0.243804325765454,0.267143901309647),
 .UNSPECIFIED.);
#173=B_SPLINE_CURVE_WITH_KNOTS('',3,(#6138,#6139,#6140,#6141,#6142,#6143,
#6144,#6145,#6146,#6147,#6148,#6149,#6150,#6151),.UNSPECIFIED.,.F.,.F.,
(4,2,2,2,2,2,4),(0.466102891398403,0.489272506433,0.524287150622646,0.559301794812291,
0.594316439001936,0.629331083191582,0.652500698226179),.UNSPECIFIED.);
#174=B_SPLINE_CURVE_WITH_KNOTS('',3,(#6156,#6157,#6158,#6159,#6160,#6161,
#6162,#6163,#6164,#6165,#6166,#6167,#6168,#6169),.UNSPECIFIED.,.F.,.F.,
(4,2,2,2,2,2,4),(0.0804140797636754,0.103753655307869,0.138766322922265,
0.173778990536662,0.208791658151058,0.243804325765454,0.267143901309648),
 .UNSPECIFIED.);
#175=B_SPLINE_CURVE_WITH_KNOTS('',3,(#6173,#6174,#6175,#6176,#6177,#6178,
#6179,#6180,#6181,#6182,#6183,#6184,#6185,#6186),.UNSPECIFIED.,.F.,.F.,
(4,2,2,2,2,2,4),(0.466102891398402,0.489272506433,0.524287150622646,0.559301794812291,
0.594316439001936,0.629331083191581,0.652500698226179),.UNSPECIFIED.);
#176=B_SPLINE_CURVE_WITH_KNOTS('',3,(#6191,#6192,#6193,#6194,#6195,#6196,
#6197,#6198,#6199,#6200,#6201,#6202,#6203,#6204),.UNSPECIFIED.,.F.,.F.,
(4,2,2,2,2,2,4),(0.0804140797636755,0.103753655307869,0.138766322922265,
0.173778990536661,0.208791658151058,0.243804325765454,0.267143901309648),
 .UNSPECIFIED.);
#177=B_SPLINE_CURVE_WITH_KNOTS('',3,(#6208,#6209,#6210,#6211,#6212,#6213,
#6214,#6215,#6216,#6217,#6218,#6219,#6220,#6221),.UNSPECIFIED.,.F.,.F.,
(4,2,2,2,2,2,4),(0.466102891398402,0.489272506433,0.524287150622645,0.55930179481229,
0.594316439001935,0.629331083191581,0.652500698226178),.UNSPECIFIED.);
#178=B_SPLINE_CURVE_WITH_KNOTS('',3,(#6226,#6227,#6228,#6229,#6230,#6231,
#6232,#6233,#6234,#6235,#6236,#6237,#6238,#6239),.UNSPECIFIED.,.F.,.F.,
(4,2,2,2,2,2,4),(0.0804140797636754,0.103753655307869,0.138766322922265,
0.173778990536662,0.208791658151058,0.243804325765454,0.267143901309648),
 .UNSPECIFIED.);
#179=B_SPLINE_CURVE_WITH_KNOTS('',3,(#6243,#6244,#6245,#6246,#6247,#6248,
#6249,#6250,#6251,#6252,#6253,#6254,#6255,#6256),.UNSPECIFIED.,.F.,.F.,
(4,2,2,2,2,2,4),(0.466102891398402,0.489272506433,0.524287150622645,0.559301794812291,
0.594316439001936,0.629331083191581,0.652500698226179),.UNSPECIFIED.);
#180=B_SPLINE_CURVE_WITH_KNOTS('',3,(#6261,#6262,#6263,#6264,#6265,#6266,
#6267,#6268,#6269,#6270,#6271,#6272,#6273,#6274),.UNSPECIFIED.,.F.,.F.,
(4,2,2,2,2,2,4),(0.0804140797636753,0.103753655307869,0.138766322922265,
0.173778990536662,0.208791658151058,0.243804325765455,0.267143901309648),
 .UNSPECIFIED.);
#181=B_SPLINE_CURVE_WITH_KNOTS('',3,(#6278,#6279,#6280,#6281,#6282,#6283,
#6284,#6285,#6286,#6287,#6288,#6289,#6290,#6291),.UNSPECIFIED.,.F.,.F.,
(4,2,2,2,2,2,4),(0.466102891398403,0.489272506433,0.524287150622645,0.559301794812291,
0.594316439001936,0.629331083191581,0.652500698226179),.UNSPECIFIED.);
#182=B_SPLINE_CURVE_WITH_KNOTS('',3,(#6296,#6297,#6298,#6299,#6300,#6301,
#6302,#6303,#6304,#6305,#6306,#6307,#6308,#6309),.UNSPECIFIED.,.F.,.F.,
(4,2,2,2,2,2,4),(0.0804140797636755,0.103753655307869,0.138766322922265,
0.173778990536662,0.208791658151058,0.243804325765455,0.267143901309648),
 .UNSPECIFIED.);
#183=B_SPLINE_CURVE_WITH_KNOTS('',3,(#6313,#6314,#6315,#6316,#6317,#6318,
#6319,#6320,#6321,#6322,#6323,#6324,#6325,#6326),.UNSPECIFIED.,.F.,.F.,
(4,2,2,2,2,2,4),(0.466102891398403,0.489272506433,0.524287150622645,0.55930179481229,
0.594316439001936,0.629331083191581,0.652500698226179),.UNSPECIFIED.);
#184=B_SPLINE_CURVE_WITH_KNOTS('',3,(#6331,#6332,#6333,#6334,#6335,#6336,
#6337,#6338,#6339,#6340,#6341,#6342,#6343,#6344),.UNSPECIFIED.,.F.,.F.,
(4,2,2,2,2,2,4),(0.0804140797636754,0.103753655307869,0.138766322922265,
0.173778990536661,0.208791658151058,0.243804325765454,0.267143901309648),
 .UNSPECIFIED.);
#185=B_SPLINE_CURVE_WITH_KNOTS('',3,(#6348,#6349,#6350,#6351,#6352,#6353,
#6354,#6355,#6356,#6357,#6358,#6359,#6360,#6361),.UNSPECIFIED.,.F.,.F.,
(4,2,2,2,2,2,4),(0.466102891398402,0.489272506433,0.524287150622645,0.55930179481229,
0.594316439001936,0.629331083191581,0.652500698226179),.UNSPECIFIED.);
#186=B_SPLINE_CURVE_WITH_KNOTS('',3,(#6366,#6367,#6368,#6369,#6370,#6371,
#6372,#6373,#6374,#6375,#6376,#6377,#6378,#6379),.UNSPECIFIED.,.F.,.F.,
(4,2,2,2,2,2,4),(0.0804140797636754,0.103753655307869,0.138766322922265,
0.173778990536662,0.208791658151058,0.243804325765454,0.267143901309648),
 .UNSPECIFIED.);
#187=B_SPLINE_CURVE_WITH_KNOTS('',3,(#6383,#6384,#6385,#6386,#6387,#6388,
#6389,#6390,#6391,#6392,#6393,#6394,#6395,#6396),.UNSPECIFIED.,.F.,.F.,
(4,2,2,2,2,2,4),(0.466102891398402,0.489272506433,0.524287150622645,0.55930179481229,
0.594316439001935,0.62933108319158,0.652500698226178),.UNSPECIFIED.);
#188=B_SPLINE_CURVE_WITH_KNOTS('',3,(#6401,#6402,#6403,#6404,#6405,#6406,
#6407,#6408,#6409,#6410,#6411,#6412,#6413,#6414),.UNSPECIFIED.,.F.,.F.,
(4,2,2,2,2,2,4),(0.0804140797636753,0.103753655307869,0.138766322922265,
0.173778990536661,0.208791658151058,0.243804325765454,0.267143901309648),
 .UNSPECIFIED.);
#189=B_SPLINE_CURVE_WITH_KNOTS('',3,(#6418,#6419,#6420,#6421,#6422,#6423,
#6424,#6425,#6426,#6427,#6428,#6429,#6430,#6431),.UNSPECIFIED.,.F.,.F.,
(4,2,2,2,2,2,4),(0.466102891398402,0.489272506432999,0.524287150622645,
0.55930179481229,0.594316439001935,0.62933108319158,0.652500698226178),
 .UNSPECIFIED.);
#190=B_SPLINE_CURVE_WITH_KNOTS('',3,(#6436,#6437,#6438,#6439,#6440,#6441,
#6442,#6443,#6444,#6445,#6446,#6447,#6448,#6449),.UNSPECIFIED.,.F.,.F.,
(4,2,2,2,2,2,4),(0.0804140797636754,0.103753655307869,0.138766322922265,
0.173778990536661,0.208791658151058,0.243804325765454,0.267143901309648),
 .UNSPECIFIED.);
#191=B_SPLINE_CURVE_WITH_KNOTS('',3,(#6453,#6454,#6455,#6456,#6457,#6458,
#6459,#6460,#6461,#6462,#6463,#6464,#6465,#6466),.UNSPECIFIED.,.F.,.F.,
(4,2,2,2,2,2,4),(0.466102891398402,0.489272506433,0.524287150622645,0.55930179481229,
0.594316439001935,0.629331083191581,0.652500698226178),.UNSPECIFIED.);
#192=B_SPLINE_CURVE_WITH_KNOTS('',3,(#6471,#6472,#6473,#6474,#6475,#6476,
#6477,#6478,#6479,#6480,#6481,#6482,#6483,#6484),.UNSPECIFIED.,.F.,.F.,
(4,2,2,2,2,2,4),(0.0804140797636754,0.103753655307869,0.138766322922265,
0.173778990536662,0.208791658151058,0.243804325765454,0.267143901309648),
 .UNSPECIFIED.);
#193=B_SPLINE_CURVE_WITH_KNOTS('',3,(#6488,#6489,#6490,#6491,#6492,#6493,
#6494,#6495,#6496,#6497,#6498,#6499,#6500,#6501),.UNSPECIFIED.,.F.,.F.,
(4,2,2,2,2,2,4),(0.466102891398403,0.489272506433,0.524287150622646,0.559301794812291,
0.594316439001936,0.629331083191581,0.652500698226179),.UNSPECIFIED.);
#194=B_SPLINE_CURVE_WITH_KNOTS('',3,(#6506,#6507,#6508,#6509,#6510,#6511,
#6512,#6513,#6514,#6515,#6516,#6517,#6518,#6519),.UNSPECIFIED.,.F.,.F.,
(4,2,2,2,2,2,4),(0.0804140797636752,0.103753655307869,0.138766322922265,
0.173778990536661,0.208791658151058,0.243804325765454,0.267143901309648),
 .UNSPECIFIED.);
#195=B_SPLINE_CURVE_WITH_KNOTS('',3,(#6523,#6524,#6525,#6526,#6527,#6528,
#6529,#6530,#6531,#6532,#6533,#6534,#6535,#6536),.UNSPECIFIED.,.F.,.F.,
(4,2,2,2,2,2,4),(0.466102891398402,0.489272506432999,0.524287150622644,
0.559301794812289,0.594316439001935,0.62933108319158,0.652500698226178),
 .UNSPECIFIED.);
#196=B_SPLINE_CURVE_WITH_KNOTS('',3,(#6541,#6542,#6543,#6544,#6545,#6546,
#6547,#6548,#6549,#6550,#6551,#6552,#6553,#6554),.UNSPECIFIED.,.F.,.F.,
(4,2,2,2,2,2,4),(0.0804140797636753,0.103753655307869,0.138766322922265,
0.173778990536662,0.208791658151058,0.243804325765455,0.267143901309648),
 .UNSPECIFIED.);
#197=B_SPLINE_CURVE_WITH_KNOTS('',3,(#6558,#6559,#6560,#6561,#6562,#6563,
#6564,#6565,#6566,#6567,#6568,#6569,#6570,#6571),.UNSPECIFIED.,.F.,.F.,
(4,2,2,2,2,2,4),(0.466102891398402,0.489272506432999,0.524287150622644,
0.55930179481229,0.594316439001935,0.62933108319158,0.652500698226178),
 .UNSPECIFIED.);
#198=B_SPLINE_CURVE_WITH_KNOTS('',3,(#6576,#6577,#6578,#6579,#6580,#6581,
#6582,#6583,#6584,#6585,#6586,#6587,#6588,#6589),.UNSPECIFIED.,.F.,.F.,
(4,2,2,2,2,2,4),(0.0804140797636755,0.103753655307869,0.138766322922265,
0.173778990536661,0.208791658151058,0.243804325765454,0.267143901309648),
 .UNSPECIFIED.);
#199=B_SPLINE_CURVE_WITH_KNOTS('',3,(#6593,#6594,#6595,#6596,#6597,#6598,
#6599,#6600,#6601,#6602,#6603,#6604,#6605,#6606),.UNSPECIFIED.,.F.,.F.,
(4,2,2,2,2,2,4),(0.466102891398403,0.489272506433,0.524287150622646,0.559301794812291,
0.594316439001936,0.629331083191581,0.652500698226179),.UNSPECIFIED.);
#200=B_SPLINE_CURVE_WITH_KNOTS('',3,(#6611,#6612,#6613,#6614,#6615,#6616,
#6617,#6618,#6619,#6620,#6621,#6622,#6623,#6624),.UNSPECIFIED.,.F.,.F.,
(4,2,2,2,2,2,4),(0.0804140797636754,0.103753655307869,0.138766322922265,
0.173778990536662,0.208791658151058,0.243804325765454,0.267143901309648),
 .UNSPECIFIED.);
#201=B_SPLINE_CURVE_WITH_KNOTS('',3,(#6628,#6629,#6630,#6631,#6632,#6633,
#6634,#6635,#6636,#6637,#6638,#6639,#6640,#6641),.UNSPECIFIED.,.F.,.F.,
(4,2,2,2,2,2,4),(0.466102891398403,0.489272506433,0.524287150622646,0.559301794812291,
0.594316439001936,0.629331083191581,0.652500698226179),.UNSPECIFIED.);
#202=B_SPLINE_CURVE_WITH_KNOTS('',3,(#6646,#6647,#6648,#6649,#6650,#6651,
#6652,#6653,#6654,#6655,#6656,#6657,#6658,#6659),.UNSPECIFIED.,.F.,.F.,
(4,2,2,2,2,2,4),(0.0804140797636755,0.103753655307869,0.138766322922265,
0.173778990536662,0.208791658151058,0.243804325765454,0.267143901309648),
 .UNSPECIFIED.);
#203=B_SPLINE_CURVE_WITH_KNOTS('',3,(#6663,#6664,#6665,#6666,#6667,#6668,
#6669,#6670,#6671,#6672,#6673,#6674,#6675,#6676),.UNSPECIFIED.,.F.,.F.,
(4,2,2,2,2,2,4),(0.466102891398403,0.489272506433,0.524287150622645,0.55930179481229,
0.594316439001935,0.62933108319158,0.652500698226178),.UNSPECIFIED.);
#204=B_SPLINE_CURVE_WITH_KNOTS('',3,(#6681,#6682,#6683,#6684,#6685,#6686,
#6687,#6688,#6689,#6690,#6691,#6692,#6693,#6694),.UNSPECIFIED.,.F.,.F.,
(4,2,2,2,2,2,4),(0.0804140797636754,0.103753655307869,0.138766322922265,
0.173778990536662,0.208791658151058,0.243804325765455,0.267143901309648),
 .UNSPECIFIED.);
#205=B_SPLINE_CURVE_WITH_KNOTS('',3,(#6698,#6699,#6700,#6701,#6702,#6703,
#6704,#6705,#6706,#6707,#6708,#6709,#6710,#6711),.UNSPECIFIED.,.F.,.F.,
(4,2,2,2,2,2,4),(0.466102891398403,0.489272506433001,0.524287150622646,
0.559301794812291,0.594316439001936,0.629331083191582,0.65250069822618),
 .UNSPECIFIED.);
#206=B_SPLINE_CURVE_WITH_KNOTS('',3,(#6716,#6717,#6718,#6719,#6720,#6721,
#6722,#6723,#6724,#6725,#6726,#6727,#6728,#6729),.UNSPECIFIED.,.F.,.F.,
(4,2,2,2,2,2,4),(0.0804140797636755,0.103753655307869,0.138766322922265,
0.173778990536661,0.208791658151058,0.243804325765455,0.267143901309648),
 .UNSPECIFIED.);
#207=B_SPLINE_CURVE_WITH_KNOTS('',3,(#6733,#6734,#6735,#6736,#6737,#6738,
#6739,#6740,#6741,#6742,#6743,#6744,#6745,#6746),.UNSPECIFIED.,.F.,.F.,
(4,2,2,2,2,2,4),(0.466102891398403,0.489272506433,0.524287150622645,0.559301794812291,
0.594316439001936,0.629331083191581,0.652500698226178),.UNSPECIFIED.);
#208=B_SPLINE_CURVE_WITH_KNOTS('',3,(#6751,#6752,#6753,#6754,#6755,#6756,
#6757,#6758,#6759,#6760,#6761,#6762,#6763,#6764),.UNSPECIFIED.,.F.,.F.,
(4,2,2,2,2,2,4),(0.0804140797636753,0.103753655307869,0.138766322922265,
0.173778990536662,0.208791658151058,0.243804325765455,0.267143901309648),
 .UNSPECIFIED.);
#209=B_SPLINE_CURVE_WITH_KNOTS('',3,(#6768,#6769,#6770,#6771,#6772,#6773,
#6774,#6775,#6776,#6777,#6778,#6779,#6780,#6781),.UNSPECIFIED.,.F.,.F.,
(4,2,2,2,2,2,4),(0.466102891398403,0.489272506433,0.524287150622646,0.559301794812291,
0.594316439001936,0.629331083191581,0.652500698226179),.UNSPECIFIED.);
#210=B_SPLINE_CURVE_WITH_KNOTS('',3,(#6786,#6787,#6788,#6789,#6790,#6791,
#6792,#6793,#6794,#6795,#6796,#6797,#6798,#6799),.UNSPECIFIED.,.F.,.F.,
(4,2,2,2,2,2,4),(0.0804140797636753,0.103753655307869,0.138766322922265,
0.173778990536662,0.208791658151058,0.243804325765455,0.267143901309648),
 .UNSPECIFIED.);
#211=B_SPLINE_CURVE_WITH_KNOTS('',3,(#6803,#6804,#6805,#6806,#6807,#6808,
#6809,#6810,#6811,#6812,#6813,#6814,#6815,#6816),.UNSPECIFIED.,.F.,.F.,
(4,2,2,2,2,2,4),(0.466102891398403,0.489272506433,0.524287150622646,0.559301794812291,
0.594316439001936,0.629331083191581,0.652500698226179),.UNSPECIFIED.);
#212=B_SPLINE_CURVE_WITH_KNOTS('',3,(#6821,#6822,#6823,#6824,#6825,#6826,
#6827,#6828,#6829,#6830,#6831,#6832,#6833,#6834),.UNSPECIFIED.,.F.,.F.,
(4,2,2,2,2,2,4),(0.0804140797636755,0.103753655307869,0.138766322922265,
0.173778990536661,0.208791658151058,0.243804325765454,0.267143901309648),
 .UNSPECIFIED.);
#213=B_SPLINE_CURVE_WITH_KNOTS('',3,(#6838,#6839,#6840,#6841,#6842,#6843,
#6844,#6845,#6846,#6847,#6848,#6849,#6850,#6851),.UNSPECIFIED.,.F.,.F.,
(4,2,2,2,2,2,4),(0.466102891398403,0.489272506433,0.524287150622646,0.559301794812291,
0.594316439001936,0.629331083191581,0.652500698226179),.UNSPECIFIED.);
#214=B_SPLINE_CURVE_WITH_KNOTS('',3,(#6856,#6857,#6858,#6859,#6860,#6861,
#6862,#6863,#6864,#6865,#6866,#6867,#6868,#6869),.UNSPECIFIED.,.F.,.F.,
(4,2,2,2,2,2,4),(0.0804140797636756,0.103753655307869,0.138766322922265,
0.173778990536662,0.208791658151058,0.243804325765454,0.267143901309648),
 .UNSPECIFIED.);
#215=B_SPLINE_CURVE_WITH_KNOTS('',3,(#6873,#6874,#6875,#6876,#6877,#6878,
#6879,#6880,#6881,#6882,#6883,#6884,#6885,#6886),.UNSPECIFIED.,.F.,.F.,
(4,2,2,2,2,2,4),(0.466102891398403,0.489272506433,0.524287150622645,0.55930179481229,
0.594316439001936,0.629331083191581,0.652500698226178),.UNSPECIFIED.);
#216=B_SPLINE_CURVE_WITH_KNOTS('',3,(#6894,#6895,#6896,#6897,#6898,#6899,
#6900,#6901),.UNSPECIFIED.,.F.,.F.,(4,2,2,4),(0.559301794812291,0.594316439001936,
0.629331083191581,0.652500698226179),.UNSPECIFIED.);
#217=B_SPLINE_CURVE_WITH_KNOTS('',3,(#6928,#6929,#6930,#6931,#6932,#6933,
#6934,#6935),.UNSPECIFIED.,.F.,.F.,(4,2,2,4),(0.466102891398403,0.489272506433001,
0.524287150622646,0.559301794812291),.UNSPECIFIED.);
#218=B_SPLINE_CURVE_WITH_KNOTS('',3,(#6990,#6991,#6992,#6993,#6994,#6995,
#6996,#6997),.UNSPECIFIED.,.F.,.F.,(4,2,2,4),(0.0804140797636754,0.103753655307869,
0.138766322922265,0.173778990536661),.UNSPECIFIED.);
#219=B_SPLINE_CURVE_WITH_KNOTS('',3,(#6998,#6999,#7000,#7001,#7002,#7003,
#7004,#7005),.UNSPECIFIED.,.F.,.F.,(4,2,2,4),(0.173778990536661,0.208791658151058,
0.243804325765454,0.267143901309647),.UNSPECIFIED.);
#220=B_SPLINE_CURVE_WITH_KNOTS('',3,(#7037,#7038,#7039,#7040,#7041,#7042,
#7043,#7044,#7045,#7046,#7047,#7048,#7049,#7050,#7051,#7052,#7053,#7054),
 .UNSPECIFIED.,.F.,.F.,(4,2,2,2,2,2,2,2,4),(0.,0.0376986977587122,0.0753973955174244,
0.11309593596243,0.150794476407437,0.188493016852443,0.226191557297449,
0.263890255056161,0.301588952814873),.UNSPECIFIED.);
#221=B_SPLINE_CURVE_WITH_KNOTS('',3,(#7057,#7058,#7059,#7060,#7061,#7062,
#7063,#7064,#7065,#7066,#7067,#7068,#7069,#7070,#7071,#7072,#7073,#7074),
 .UNSPECIFIED.,.F.,.F.,(4,2,2,2,2,2,2,2,4),(-0.301588952814873,-0.263890255056161,
-0.226191557297449,-0.188493016852443,-0.150794476407437,-0.113095935962431,
-0.0753973955174246,-0.0376986977587124,0.),.UNSPECIFIED.);
#222=B_SPLINE_CURVE_WITH_KNOTS('',3,(#7085,#7086,#7087,#7088,#7089,#7090,
#7091,#7092,#7093,#7094),.UNSPECIFIED.,.F.,.F.,(4,2,2,2,4),(-0.150763619405615,
-0.113072757903898,-0.0753818964021818,-0.037690948201091,0.),
 .UNSPECIFIED.);
#223=B_SPLINE_CURVE_WITH_KNOTS('',3,(#7095,#7096,#7097,#7098,#7099,#7100,
#7101,#7102,#7103,#7104),.UNSPECIFIED.,.F.,.F.,(4,2,2,2,4),(-0.30152723881123,
-0.263836290610139,-0.226145342409048,-0.188454480907332,-0.150763619405615),
 .UNSPECIFIED.);
#224=B_SPLINE_CURVE_WITH_KNOTS('',3,(#7108,#7109,#7110,#7111,#7112,#7113,
#7114,#7115,#7116,#7117),.UNSPECIFIED.,.F.,.F.,(4,2,2,2,4),(0.,0.037690948201091,
0.075381896402182,0.113072757903899,0.150763619405615),.UNSPECIFIED.);
#225=B_SPLINE_CURVE_WITH_KNOTS('',3,(#7119,#7120,#7121,#7122,#7123,#7124,
#7125,#7126,#7127,#7128),.UNSPECIFIED.,.F.,.F.,(4,2,2,2,4),(0.452290858216846,
0.489981719718562,0.527672581220279,0.56536352942137,0.603054477622461),
 .UNSPECIFIED.);
#226=B_SPLINE_CURVE_WITH_KNOTS('',3,(#7132,#7133,#7134,#7135,#7136,#7137,
#7138,#7139,#7140,#7141,#7142,#7143,#7144,#7145,#7146,#7147,#7148,#7149),
 .UNSPECIFIED.,.F.,.F.,(4,2,2,2,2,2,2,2,4),(0.150763619405615,0.188454480907332,
0.226145342409048,0.263836290610139,0.30152723881123,0.339218187012321,
0.376909135213412,0.414599996715129,0.452290858216846),.UNSPECIFIED.);
#227=B_SPLINE_CURVE_WITH_KNOTS('',3,(#7157,#7158,#7159,#7160,#7161,#7162,
#7163,#7164,#7165,#7166),.UNSPECIFIED.,.F.,.F.,(4,2,2,2,4),(0.150763619405615,
0.188454480907332,0.226145342409048,0.263836290610139,0.30152723881123),
 .UNSPECIFIED.);
#228=B_SPLINE_CURVE_WITH_KNOTS('',3,(#7167,#7168,#7169,#7170,#7171,#7172,
#7173,#7174,#7175,#7176),.UNSPECIFIED.,.F.,.F.,(4,2,2,2,4),(0.,0.037690948201091,
0.075381896402182,0.113072757903899,0.150763619405615),.UNSPECIFIED.);
#229=LINE('',#4676,#389);
#230=LINE('',#4695,#390);
#231=LINE('',#4711,#391);
#232=LINE('',#4730,#392);
#233=LINE('',#4746,#393);
#234=LINE('',#4765,#394);
#235=LINE('',#4781,#395);
#236=LINE('',#4800,#396);
#237=LINE('',#4816,#397);
#238=LINE('',#4835,#398);
#239=LINE('',#4851,#399);
#240=LINE('',#4870,#400);
#241=LINE('',#4886,#401);
#242=LINE('',#4905,#402);
#243=LINE('',#4921,#403);
#244=LINE('',#4940,#404);
#245=LINE('',#4956,#405);
#246=LINE('',#4975,#406);
#247=LINE('',#4991,#407);
#248=LINE('',#5010,#408);
#249=LINE('',#5026,#409);
#250=LINE('',#5045,#410);
#251=LINE('',#5061,#411);
#252=LINE('',#5080,#412);
#253=LINE('',#5096,#413);
#254=LINE('',#5115,#414);
#255=LINE('',#5131,#415);
#256=LINE('',#5150,#416);
#257=LINE('',#5166,#417);
#258=LINE('',#5185,#418);
#259=LINE('',#5201,#419);
#260=LINE('',#5220,#420);
#261=LINE('',#5236,#421);
#262=LINE('',#5255,#422);
#263=LINE('',#5271,#423);
#264=LINE('',#5290,#424);
#265=LINE('',#5306,#425);
#266=LINE('',#5325,#426);
#267=LINE('',#5341,#427);
#268=LINE('',#5360,#428);
#269=LINE('',#5376,#429);
#270=LINE('',#5395,#430);
#271=LINE('',#5411,#431);
#272=LINE('',#5430,#432);
#273=LINE('',#5446,#433);
#274=LINE('',#5465,#434);
#275=LINE('',#5481,#435);
#276=LINE('',#5500,#436);
#277=LINE('',#5516,#437);
#278=LINE('',#5521,#438);
#279=LINE('',#5568,#439);
#280=LINE('',#5571,#440);
#281=LINE('',#5637,#441);
#282=LINE('',#5644,#442);
#283=LINE('',#5661,#443);
#284=LINE('',#5664,#444);
#285=LINE('',#5667,#445);
#286=LINE('',#5673,#446);
#287=LINE('',#5674,#447);
#288=LINE('',#5684,#448);
#289=LINE('',#5687,#449);
#290=LINE('',#5688,#450);
#291=LINE('',#5696,#451);
#292=LINE('',#5721,#452);
#293=LINE('',#5726,#453);
#294=LINE('',#5751,#454);
#295=LINE('',#5756,#455);
#296=LINE('',#5781,#456);
#297=LINE('',#5786,#457);
#298=LINE('',#5811,#458);
#299=LINE('',#5816,#459);
#300=LINE('',#5845,#460);
#301=LINE('',#5850,#461);
#302=LINE('',#5875,#462);
#303=LINE('',#5880,#463);
#304=LINE('',#5905,#464);
#305=LINE('',#5910,#465);
#306=LINE('',#5935,#466);
#307=LINE('',#5940,#467);
#308=LINE('',#5965,#468);
#309=LINE('',#5986,#469);
#310=LINE('',#6039,#470);
#311=LINE('',#6045,#471);
#312=LINE('',#6066,#472);
#313=LINE('',#6082,#473);
#314=LINE('',#6101,#474);
#315=LINE('',#6117,#475);
#316=LINE('',#6136,#476);
#317=LINE('',#6152,#477);
#318=LINE('',#6171,#478);
#319=LINE('',#6187,#479);
#320=LINE('',#6206,#480);
#321=LINE('',#6222,#481);
#322=LINE('',#6241,#482);
#323=LINE('',#6257,#483);
#324=LINE('',#6276,#484);
#325=LINE('',#6292,#485);
#326=LINE('',#6311,#486);
#327=LINE('',#6327,#487);
#328=LINE('',#6346,#488);
#329=LINE('',#6362,#489);
#330=LINE('',#6381,#490);
#331=LINE('',#6397,#491);
#332=LINE('',#6416,#492);
#333=LINE('',#6432,#493);
#334=LINE('',#6451,#494);
#335=LINE('',#6467,#495);
#336=LINE('',#6486,#496);
#337=LINE('',#6502,#497);
#338=LINE('',#6521,#498);
#339=LINE('',#6537,#499);
#340=LINE('',#6556,#500);
#341=LINE('',#6572,#501);
#342=LINE('',#6591,#502);
#343=LINE('',#6607,#503);
#344=LINE('',#6626,#504);
#345=LINE('',#6642,#505);
#346=LINE('',#6661,#506);
#347=LINE('',#6677,#507);
#348=LINE('',#6696,#508);
#349=LINE('',#6712,#509);
#350=LINE('',#6731,#510);
#351=LINE('',#6747,#511);
#352=LINE('',#6766,#512);
#353=LINE('',#6782,#513);
#354=LINE('',#6801,#514);
#355=LINE('',#6817,#515);
#356=LINE('',#6836,#516);
#357=LINE('',#6852,#517);
#358=LINE('',#6871,#518);
#359=LINE('',#6887,#519);
#360=LINE('',#6892,#520);
#361=LINE('',#6939,#521);
#362=LINE('',#6942,#522);
#363=LINE('',#7009,#523);
#364=LINE('',#7017,#524);
#365=LINE('',#7020,#525);
#366=LINE('',#7029,#526);
#367=LINE('',#7035,#527);
#368=LINE('',#7056,#528);
#369=LINE('',#7077,#529);
#370=LINE('',#7079,#530);
#371=LINE('',#7080,#531);
#372=LINE('',#7083,#532);
#373=LINE('',#7130,#533);
#374=LINE('',#7153,#534);
#375=LINE('',#7154,#535);
#376=LINE('',#7183,#536);
#377=LINE('',#7191,#537);
#378=LINE('',#7199,#538);
#379=LINE('',#7200,#539);
#380=LINE('',#7202,#540);
#381=LINE('',#7214,#541);
#382=LINE('',#7232,#542);
#383=LINE('',#7238,#543);
#384=LINE('',#7246,#544);
#385=LINE('',#7251,#545);
#386=LINE('',#7263,#546);
#387=LINE('',#7272,#547);
#388=LINE('',#7278,#548);
#389=VECTOR('',#3744,10.5057959473896);
#390=VECTOR('',#3747,10.);
#391=VECTOR('',#3748,10.);
#392=VECTOR('',#3751,10.);
#393=VECTOR('',#3752,10.);
#394=VECTOR('',#3755,10.);
#395=VECTOR('',#3756,10.);
#396=VECTOR('',#3759,10.);
#397=VECTOR('',#3760,10.);
#398=VECTOR('',#3763,10.);
#399=VECTOR('',#3764,10.);
#400=VECTOR('',#3767,10.);
#401=VECTOR('',#3768,10.);
#402=VECTOR('',#3771,10.);
#403=VECTOR('',#3772,10.);
#404=VECTOR('',#3775,10.);
#405=VECTOR('',#3776,10.);
#406=VECTOR('',#3779,10.);
#407=VECTOR('',#3780,10.);
#408=VECTOR('',#3783,10.);
#409=VECTOR('',#3784,10.);
#410=VECTOR('',#3787,10.);
#411=VECTOR('',#3788,10.);
#412=VECTOR('',#3791,10.);
#413=VECTOR('',#3792,10.);
#414=VECTOR('',#3795,10.);
#415=VECTOR('',#3796,10.);
#416=VECTOR('',#3799,10.);
#417=VECTOR('',#3800,10.);
#418=VECTOR('',#3803,10.);
#419=VECTOR('',#3804,10.);
#420=VECTOR('',#3807,10.);
#421=VECTOR('',#3808,10.);
#422=VECTOR('',#3811,10.);
#423=VECTOR('',#3812,10.);
#424=VECTOR('',#3815,10.);
#425=VECTOR('',#3816,10.);
#426=VECTOR('',#3819,10.);
#427=VECTOR('',#3820,10.);
#428=VECTOR('',#3823,10.);
#429=VECTOR('',#3824,10.);
#430=VECTOR('',#3827,10.);
#431=VECTOR('',#3828,10.);
#432=VECTOR('',#3831,10.);
#433=VECTOR('',#3832,10.);
#434=VECTOR('',#3835,10.);
#435=VECTOR('',#3836,10.);
#436=VECTOR('',#3839,10.);
#437=VECTOR('',#3840,10.);
#438=VECTOR('',#3845,10.7746348408465);
#439=VECTOR('',#3900,10.);
#440=VECTOR('',#3903,10.);
#441=VECTOR('',#4000,10.765215394118);
#442=VECTOR('',#4011,9.50579594738959);
#443=VECTOR('',#4022,10.);
#444=VECTOR('',#4025,10.);
#445=VECTOR('',#4028,10.);
#446=VECTOR('',#4029,10.);
#447=VECTOR('',#4030,10.);
#448=VECTOR('',#4039,10.);
#449=VECTOR('',#4042,10.);
#450=VECTOR('',#4043,10.);
#451=VECTOR('',#4054,10.);
#452=VECTOR('',#4055,10.);
#453=VECTOR('',#4060,10.);
#454=VECTOR('',#4061,10.);
#455=VECTOR('',#4066,10.);
#456=VECTOR('',#4067,10.);
#457=VECTOR('',#4072,10.);
#458=VECTOR('',#4073,10.);
#459=VECTOR('',#4078,10.);
#460=VECTOR('',#4079,10.);
#461=VECTOR('',#4084,10.);
#462=VECTOR('',#4085,10.);
#463=VECTOR('',#4090,10.);
#464=VECTOR('',#4091,10.);
#465=VECTOR('',#4096,10.);
#466=VECTOR('',#4097,10.);
#467=VECTOR('',#4102,10.);
#468=VECTOR('',#4103,10.);
#469=VECTOR('',#4136,10.);
#470=VECTOR('',#4179,10.);
#471=VECTOR('',#4188,1.);
#472=VECTOR('',#4195,10.);
#473=VECTOR('',#4196,10.);
#474=VECTOR('',#4199,10.);
#475=VECTOR('',#4200,10.);
#476=VECTOR('',#4203,10.);
#477=VECTOR('',#4204,10.);
#478=VECTOR('',#4207,10.);
#479=VECTOR('',#4208,10.);
#480=VECTOR('',#4211,10.);
#481=VECTOR('',#4212,10.);
#482=VECTOR('',#4215,10.);
#483=VECTOR('',#4216,10.);
#484=VECTOR('',#4219,10.);
#485=VECTOR('',#4220,10.);
#486=VECTOR('',#4223,10.);
#487=VECTOR('',#4224,10.);
#488=VECTOR('',#4227,10.);
#489=VECTOR('',#4228,10.);
#490=VECTOR('',#4231,10.);
#491=VECTOR('',#4232,10.);
#492=VECTOR('',#4235,10.);
#493=VECTOR('',#4236,10.);
#494=VECTOR('',#4239,10.);
#495=VECTOR('',#4240,10.);
#496=VECTOR('',#4243,10.);
#497=VECTOR('',#4244,10.);
#498=VECTOR('',#4247,10.);
#499=VECTOR('',#4248,10.);
#500=VECTOR('',#4251,10.);
#501=VECTOR('',#4252,10.);
#502=VECTOR('',#4255,10.);
#503=VECTOR('',#4256,10.);
#504=VECTOR('',#4259,10.);
#505=VECTOR('',#4260,10.);
#506=VECTOR('',#4263,10.);
#507=VECTOR('',#4264,10.);
#508=VECTOR('',#4267,10.);
#509=VECTOR('',#4268,10.);
#510=VECTOR('',#4271,10.);
#511=VECTOR('',#4272,10.);
#512=VECTOR('',#4275,10.);
#513=VECTOR('',#4276,10.);
#514=VECTOR('',#4279,10.);
#515=VECTOR('',#4280,10.);
#516=VECTOR('',#4283,10.);
#517=VECTOR('',#4284,10.);
#518=VECTOR('',#4287,10.);
#519=VECTOR('',#4288,10.);
#520=VECTOR('',#4293,10.265215394118);
#521=VECTOR('',#4348,10.);
#522=VECTOR('',#4351,10.);
#523=VECTOR('',#4448,9.50579594738959);
#524=VECTOR('',#4459,9.50579594738959);
#525=VECTOR('',#4464,10.265215394118);
#526=VECTOR('',#4475,9.50579594738959);
#527=VECTOR('',#4480,10.);
#528=VECTOR('',#4481,10.);
#529=VECTOR('',#4484,10.);
#530=VECTOR('',#4485,10.);
#531=VECTOR('',#4486,10.);
#532=VECTOR('',#4489,10.);
#533=VECTOR('',#4492,1.);
#534=VECTOR('',#4499,10.);
#535=VECTOR('',#4500,10.);
#536=VECTOR('',#4509,4.47286361298787);
#537=VECTOR('',#4520,4.72286361298787);
#538=VECTOR('',#4531,11.0246348408465);
#539=VECTOR('',#4532,11.0246348408465);
#540=VECTOR('',#4533,11.0246348408465);
#541=VECTOR('',#4552,3.72286361298787);
#542=VECTOR('',#4575,1.51706056234455);
#543=VECTOR('',#4582,3.47286361298787);
#544=VECTOR('',#4593,3.72286361298787);
#545=VECTOR('',#4600,1.51706056234455);
#546=VECTOR('',#4615,2.);
#547=VECTOR('',#4628,3.72286361298787);
#548=VECTOR('',#4635,5.22286361298787);
#549=CYLINDRICAL_SURFACE('',#3343,10.5057959473896);
#550=CYLINDRICAL_SURFACE('',#3345,0.999999999999999);
#551=CYLINDRICAL_SURFACE('',#3346,0.999999999999999);
#552=CYLINDRICAL_SURFACE('',#3347,0.999999999999999);
#553=CYLINDRICAL_SURFACE('',#3348,0.999999999999999);
#554=CYLINDRICAL_SURFACE('',#3349,0.999999999999999);
#555=CYLINDRICAL_SURFACE('',#3350,0.999999999999999);
#556=CYLINDRICAL_SURFACE('',#3351,0.999999999999999);
#557=CYLINDRICAL_SURFACE('',#3352,0.999999999999999);
#558=CYLINDRICAL_SURFACE('',#3353,0.999999999999999);
#559=CYLINDRICAL_SURFACE('',#3354,0.999999999999999);
#560=CYLINDRICAL_SURFACE('',#3355,0.999999999999999);
#561=CYLINDRICAL_SURFACE('',#3356,0.999999999999999);
#562=CYLINDRICAL_SURFACE('',#3357,0.999999999999999);
#563=CYLINDRICAL_SURFACE('',#3358,0.999999999999999);
#564=CYLINDRICAL_SURFACE('',#3359,0.999999999999999);
#565=CYLINDRICAL_SURFACE('',#3360,0.999999999999999);
#566=CYLINDRICAL_SURFACE('',#3361,0.999999999999999);
#567=CYLINDRICAL_SURFACE('',#3362,0.999999999999999);
#568=CYLINDRICAL_SURFACE('',#3363,0.999999999999999);
#569=CYLINDRICAL_SURFACE('',#3364,0.999999999999999);
#570=CYLINDRICAL_SURFACE('',#3365,0.999999999999999);
#571=CYLINDRICAL_SURFACE('',#3366,0.999999999999999);
#572=CYLINDRICAL_SURFACE('',#3367,0.999999999999999);
#573=CYLINDRICAL_SURFACE('',#3368,0.999999999999999);
#574=CYLINDRICAL_SURFACE('',#3396,11.0246348408465);
#575=CYLINDRICAL_SURFACE('',#3398,11.0246348408465);
#576=CYLINDRICAL_SURFACE('',#3400,11.0246348408465);
#577=CYLINDRICAL_SURFACE('',#3402,11.0246348408465);
#578=CYLINDRICAL_SURFACE('',#3404,11.0246348408465);
#579=CYLINDRICAL_SURFACE('',#3406,11.0246348408465);
#580=CYLINDRICAL_SURFACE('',#3408,11.0246348408465);
#581=CYLINDRICAL_SURFACE('',#3410,11.0246348408465);
#582=CYLINDRICAL_SURFACE('',#3412,11.0246348408465);
#583=CYLINDRICAL_SURFACE('',#3414,11.0246348408465);
#584=CYLINDRICAL_SURFACE('',#3416,11.0246348408465);
#585=CYLINDRICAL_SURFACE('',#3418,11.0246348408465);
#586=CYLINDRICAL_SURFACE('',#3420,11.0246348408465);
#587=CYLINDRICAL_SURFACE('',#3422,11.0246348408465);
#588=CYLINDRICAL_SURFACE('',#3424,11.0246348408465);
#589=CYLINDRICAL_SURFACE('',#3426,11.0246348408465);
#590=CYLINDRICAL_SURFACE('',#3428,11.0246348408465);
#591=CYLINDRICAL_SURFACE('',#3430,11.0246348408465);
#592=CYLINDRICAL_SURFACE('',#3432,11.0246348408465);
#593=CYLINDRICAL_SURFACE('',#3434,11.0246348408465);
#594=CYLINDRICAL_SURFACE('',#3436,11.0246348408465);
#595=CYLINDRICAL_SURFACE('',#3438,11.0246348408465);
#596=CYLINDRICAL_SURFACE('',#3440,11.0246348408465);
#597=CYLINDRICAL_SURFACE('',#3442,11.0246348408465);
#598=CYLINDRICAL_SURFACE('',#3444,0.999999999999999);
#599=CYLINDRICAL_SURFACE('',#3447,11.0246348408465);
#600=CYLINDRICAL_SURFACE('',#3451,9.50579594738959);
#601=CYLINDRICAL_SURFACE('',#3462,6.22286361298787);
#602=CYLINDRICAL_SURFACE('',#3464,4.72286361298787);
#603=CYLINDRICAL_SURFACE('',#3468,0.5);
#604=CYLINDRICAL_SURFACE('',#3470,0.5);
#605=CYLINDRICAL_SURFACE('',#3472,0.500000000000001);
#606=CYLINDRICAL_SURFACE('',#3474,0.5);
#607=CYLINDRICAL_SURFACE('',#3476,0.5);
#608=CYLINDRICAL_SURFACE('',#3478,0.5);
#609=CYLINDRICAL_SURFACE('',#3480,0.5);
#610=CYLINDRICAL_SURFACE('',#3482,0.5);
#611=CYLINDRICAL_SURFACE('',#3484,0.5);
#612=CYLINDRICAL_SURFACE('',#3499,2.);
#613=CYLINDRICAL_SURFACE('',#3501,2.);
#614=CYLINDRICAL_SURFACE('',#3503,2.);
#615=CYLINDRICAL_SURFACE('',#3505,2.);
#616=CYLINDRICAL_SURFACE('',#3507,2.);
#617=CYLINDRICAL_SURFACE('',#3509,2.);
#618=CYLINDRICAL_SURFACE('',#3511,2.);
#619=CYLINDRICAL_SURFACE('',#3513,2.);
#620=CYLINDRICAL_SURFACE('',#3515,2.);
#621=CYLINDRICAL_SURFACE('',#3521,0.5);
#622=CYLINDRICAL_SURFACE('',#3522,2.);
#623=CYLINDRICAL_SURFACE('',#3524,1.);
#624=CYLINDRICAL_SURFACE('',#3528,0.999999999999999);
#625=CYLINDRICAL_SURFACE('',#3529,0.999999999999999);
#626=CYLINDRICAL_SURFACE('',#3530,0.999999999999999);
#627=CYLINDRICAL_SURFACE('',#3531,0.999999999999999);
#628=CYLINDRICAL_SURFACE('',#3532,0.999999999999999);
#629=CYLINDRICAL_SURFACE('',#3533,0.999999999999999);
#630=CYLINDRICAL_SURFACE('',#3534,0.999999999999999);
#631=CYLINDRICAL_SURFACE('',#3535,0.999999999999999);
#632=CYLINDRICAL_SURFACE('',#3536,0.999999999999999);
#633=CYLINDRICAL_SURFACE('',#3537,0.999999999999999);
#634=CYLINDRICAL_SURFACE('',#3538,0.999999999999999);
#635=CYLINDRICAL_SURFACE('',#3539,0.999999999999999);
#636=CYLINDRICAL_SURFACE('',#3540,0.999999999999999);
#637=CYLINDRICAL_SURFACE('',#3541,0.999999999999999);
#638=CYLINDRICAL_SURFACE('',#3542,0.999999999999999);
#639=CYLINDRICAL_SURFACE('',#3543,0.999999999999999);
#640=CYLINDRICAL_SURFACE('',#3544,0.999999999999999);
#641=CYLINDRICAL_SURFACE('',#3545,0.999999999999999);
#642=CYLINDRICAL_SURFACE('',#3546,0.999999999999999);
#643=CYLINDRICAL_SURFACE('',#3547,0.999999999999999);
#644=CYLINDRICAL_SURFACE('',#3548,0.999999999999999);
#645=CYLINDRICAL_SURFACE('',#3549,0.999999999999999);
#646=CYLINDRICAL_SURFACE('',#3550,0.999999999999999);
#647=CYLINDRICAL_SURFACE('',#3551,0.999999999999999);
#648=CYLINDRICAL_SURFACE('',#3579,11.0246348408465);
#649=CYLINDRICAL_SURFACE('',#3581,11.0246348408465);
#650=CYLINDRICAL_SURFACE('',#3583,11.0246348408465);
#651=CYLINDRICAL_SURFACE('',#3585,11.0246348408465);
#652=CYLINDRICAL_SURFACE('',#3587,11.0246348408465);
#653=CYLINDRICAL_SURFACE('',#3589,11.0246348408465);
#654=CYLINDRICAL_SURFACE('',#3591,11.0246348408465);
#655=CYLINDRICAL_SURFACE('',#3593,11.0246348408465);
#656=CYLINDRICAL_SURFACE('',#3595,11.0246348408465);
#657=CYLINDRICAL_SURFACE('',#3597,11.0246348408465);
#658=CYLINDRICAL_SURFACE('',#3599,11.0246348408465);
#659=CYLINDRICAL_SURFACE('',#3601,11.0246348408465);
#660=CYLINDRICAL_SURFACE('',#3603,11.0246348408465);
#661=CYLINDRICAL_SURFACE('',#3605,11.0246348408465);
#662=CYLINDRICAL_SURFACE('',#3607,11.0246348408465);
#663=CYLINDRICAL_SURFACE('',#3609,11.0246348408465);
#664=CYLINDRICAL_SURFACE('',#3611,11.0246348408465);
#665=CYLINDRICAL_SURFACE('',#3613,11.0246348408465);
#666=CYLINDRICAL_SURFACE('',#3615,11.0246348408465);
#667=CYLINDRICAL_SURFACE('',#3617,11.0246348408465);
#668=CYLINDRICAL_SURFACE('',#3619,11.0246348408465);
#669=CYLINDRICAL_SURFACE('',#3621,11.0246348408465);
#670=CYLINDRICAL_SURFACE('',#3623,11.0246348408465);
#671=CYLINDRICAL_SURFACE('',#3625,11.0246348408465);
#672=CYLINDRICAL_SURFACE('',#3627,0.999999999999999);
#673=CYLINDRICAL_SURFACE('',#3628,9.50579594738959);
#674=CYLINDRICAL_SURFACE('',#3633,9.50579594738959);
#675=CYLINDRICAL_SURFACE('',#3637,11.0246348408465);
#676=CYLINDRICAL_SURFACE('',#3639,9.50579594738959);
#677=CYLINDRICAL_SURFACE('',#3645,1.);
#678=CYLINDRICAL_SURFACE('',#3646,1.);
#679=CYLINDRICAL_SURFACE('',#3650,1.);
#680=CYLINDRICAL_SURFACE('',#3657,4.72286361298787);
#681=CYLINDRICAL_SURFACE('',#3663,11.0246348408465);
#682=CYLINDRICAL_SURFACE('',#3672,3.72286361298787);
#683=CYLINDRICAL_SURFACE('',#3683,1.51706056234455);
#684=CYLINDRICAL_SURFACE('',#3690,3.72286361298787);
#685=CYLINDRICAL_SURFACE('',#3694,1.51706056234455);
#686=CYLINDRICAL_SURFACE('',#3700,2.);
#687=CYLINDRICAL_SURFACE('',#3706,3.72286361298787);
#688=CYLINDRICAL_SURFACE('',#3709,5.22286361298787);
#689=FACE_BOUND('',#912,.T.);
#690=FACE_BOUND('',#987,.T.);
#691=FACE_BOUND('',#1060,.T.);
#692=FACE_BOUND('',#1069,.T.);
#693=FACE_BOUND('',#1074,.T.);
#694=FACE_BOUND('',#1077,.T.);
#695=FACE_BOUND('',#1079,.T.);
#696=FACE_BOUND('',#1083,.T.);
#697=FACE_BOUND('',#1088,.T.);
#698=FACE_BOUND('',#1100,.T.);
#699=FACE_BOUND('',#1102,.T.);
#700=PLANE('',#3341);
#701=PLANE('',#3448);
#702=PLANE('',#3449);
#703=PLANE('',#3456);
#704=PLANE('',#3458);
#705=PLANE('',#3463);
#706=PLANE('',#3466);
#707=PLANE('',#3486);
#708=PLANE('',#3523);
#709=PLANE('',#3526);
#710=PLANE('',#3630);
#711=PLANE('',#3631);
#712=PLANE('',#3644);
#713=PLANE('',#3648);
#714=PLANE('',#3649);
#715=PLANE('',#3655);
#716=PLANE('',#3665);
#717=PLANE('',#3669);
#718=PLANE('',#3670);
#719=PLANE('',#3679);
#720=PLANE('',#3681);
#721=PLANE('',#3688);
#722=PLANE('',#3692);
#723=PLANE('',#3695);
#724=PLANE('',#3703);
#725=PLANE('',#3704);
#726=PLANE('',#3712);
#727=PLANE('',#3713);
#728=FACE_OUTER_BOUND('',#910,.T.);
#729=FACE_OUTER_BOUND('',#911,.T.);
#730=FACE_OUTER_BOUND('',#913,.T.);
#731=FACE_OUTER_BOUND('',#914,.T.);
#732=FACE_OUTER_BOUND('',#915,.T.);
#733=FACE_OUTER_BOUND('',#916,.T.);
#734=FACE_OUTER_BOUND('',#917,.T.);
#735=FACE_OUTER_BOUND('',#918,.T.);
#736=FACE_OUTER_BOUND('',#919,.T.);
#737=FACE_OUTER_BOUND('',#920,.T.);
#738=FACE_OUTER_BOUND('',#921,.T.);
#739=FACE_OUTER_BOUND('',#922,.T.);
#740=FACE_OUTER_BOUND('',#923,.T.);
#741=FACE_OUTER_BOUND('',#924,.T.);
#742=FACE_OUTER_BOUND('',#925,.T.);
#743=FACE_OUTER_BOUND('',#926,.T.);
#744=FACE_OUTER_BOUND('',#927,.T.);
#745=FACE_OUTER_BOUND('',#928,.T.);
#746=FACE_OUTER_BOUND('',#929,.T.);
#747=FACE_OUTER_BOUND('',#930,.T.);
#748=FACE_OUTER_BOUND('',#931,.T.);
#749=FACE_OUTER_BOUND('',#932,.T.);
#750=FACE_OUTER_BOUND('',#933,.T.);
#751=FACE_OUTER_BOUND('',#934,.T.);
#752=FACE_OUTER_BOUND('',#935,.T.);
#753=FACE_OUTER_BOUND('',#936,.T.);
#754=FACE_OUTER_BOUND('',#937,.T.);
#755=FACE_OUTER_BOUND('',#938,.T.);
#756=FACE_OUTER_BOUND('',#939,.T.);
#757=FACE_OUTER_BOUND('',#940,.T.);
#758=FACE_OUTER_BOUND('',#941,.T.);
#759=FACE_OUTER_BOUND('',#942,.T.);
#760=FACE_OUTER_BOUND('',#943,.T.);
#761=FACE_OUTER_BOUND('',#944,.T.);
#762=FACE_OUTER_BOUND('',#945,.T.);
#763=FACE_OUTER_BOUND('',#946,.T.);
#764=FACE_OUTER_BOUND('',#947,.T.);
#765=FACE_OUTER_BOUND('',#948,.T.);
#766=FACE_OUTER_BOUND('',#949,.T.);
#767=FACE_OUTER_BOUND('',#950,.T.);
#768=FACE_OUTER_BOUND('',#951,.T.);
#769=FACE_OUTER_BOUND('',#952,.T.);
#770=FACE_OUTER_BOUND('',#953,.T.);
#771=FACE_OUTER_BOUND('',#954,.T.);
#772=FACE_OUTER_BOUND('',#955,.T.);
#773=FACE_OUTER_BOUND('',#956,.T.);
#774=FACE_OUTER_BOUND('',#957,.T.);
#775=FACE_OUTER_BOUND('',#958,.T.);
#776=FACE_OUTER_BOUND('',#959,.T.);
#777=FACE_OUTER_BOUND('',#960,.T.);
#778=FACE_OUTER_BOUND('',#961,.T.);
#779=FACE_OUTER_BOUND('',#962,.T.);
#780=FACE_OUTER_BOUND('',#963,.T.);
#781=FACE_OUTER_BOUND('',#964,.T.);
#782=FACE_OUTER_BOUND('',#965,.T.);
#783=FACE_OUTER_BOUND('',#966,.T.);
#784=FACE_OUTER_BOUND('',#967,.T.);
#785=FACE_OUTER_BOUND('',#968,.T.);
#786=FACE_OUTER_BOUND('',#969,.T.);
#787=FACE_OUTER_BOUND('',#970,.T.);
#788=FACE_OUTER_BOUND('',#971,.T.);
#789=FACE_OUTER_BOUND('',#972,.T.);
#790=FACE_OUTER_BOUND('',#973,.T.);
#791=FACE_OUTER_BOUND('',#974,.T.);
#792=FACE_OUTER_BOUND('',#975,.T.);
#793=FACE_OUTER_BOUND('',#976,.T.);
#794=FACE_OUTER_BOUND('',#977,.T.);
#795=FACE_OUTER_BOUND('',#978,.T.);
#796=FACE_OUTER_BOUND('',#979,.T.);
#797=FACE_OUTER_BOUND('',#980,.T.);
#798=FACE_OUTER_BOUND('',#981,.T.);
#799=FACE_OUTER_BOUND('',#982,.T.);
#800=FACE_OUTER_BOUND('',#983,.T.);
#801=FACE_OUTER_BOUND('',#984,.T.);
#802=FACE_OUTER_BOUND('',#985,.T.);
#803=FACE_OUTER_BOUND('',#986,.T.);
#804=FACE_OUTER_BOUND('',#988,.T.);
#805=FACE_OUTER_BOUND('',#989,.T.);
#806=FACE_OUTER_BOUND('',#990,.T.);
#807=FACE_OUTER_BOUND('',#991,.T.);
#808=FACE_OUTER_BOUND('',#992,.T.);
#809=FACE_OUTER_BOUND('',#993,.T.);
#810=FACE_OUTER_BOUND('',#994,.T.);
#811=FACE_OUTER_BOUND('',#995,.T.);
#812=FACE_OUTER_BOUND('',#996,.T.);
#813=FACE_OUTER_BOUND('',#997,.T.);
#814=FACE_OUTER_BOUND('',#998,.T.);
#815=FACE_OUTER_BOUND('',#999,.T.);
#816=FACE_OUTER_BOUND('',#1000,.T.);
#817=FACE_OUTER_BOUND('',#1001,.T.);
#818=FACE_OUTER_BOUND('',#1002,.T.);
#819=FACE_OUTER_BOUND('',#1003,.T.);
#820=FACE_OUTER_BOUND('',#1004,.T.);
#821=FACE_OUTER_BOUND('',#1005,.T.);
#822=FACE_OUTER_BOUND('',#1006,.T.);
#823=FACE_OUTER_BOUND('',#1007,.T.);
#824=FACE_OUTER_BOUND('',#1008,.T.);
#825=FACE_OUTER_BOUND('',#1009,.T.);
#826=FACE_OUTER_BOUND('',#1010,.T.);
#827=FACE_OUTER_BOUND('',#1011,.T.);
#828=FACE_OUTER_BOUND('',#1012,.T.);
#829=FACE_OUTER_BOUND('',#1013,.T.);
#830=FACE_OUTER_BOUND('',#1014,.T.);
#831=FACE_OUTER_BOUND('',#1015,.T.);
#832=FACE_OUTER_BOUND('',#1016,.T.);
#833=FACE_OUTER_BOUND('',#1017,.T.);
#834=FACE_OUTER_BOUND('',#1018,.T.);
#835=FACE_OUTER_BOUND('',#1019,.T.);
#836=FACE_OUTER_BOUND('',#1020,.T.);
#837=FACE_OUTER_BOUND('',#1021,.T.);
#838=FACE_OUTER_BOUND('',#1022,.T.);
#839=FACE_OUTER_BOUND('',#1023,.T.);
#840=FACE_OUTER_BOUND('',#1024,.T.);
#841=FACE_OUTER_BOUND('',#1025,.T.);
#842=FACE_OUTER_BOUND('',#1026,.T.);
#843=FACE_OUTER_BOUND('',#1027,.T.);
#844=FACE_OUTER_BOUND('',#1028,.T.);
#845=FACE_OUTER_BOUND('',#1029,.T.);
#846=FACE_OUTER_BOUND('',#1030,.T.);
#847=FACE_OUTER_BOUND('',#1031,.T.);
#848=FACE_OUTER_BOUND('',#1032,.T.);
#849=FACE_OUTER_BOUND('',#1033,.T.);
#850=FACE_OUTER_BOUND('',#1034,.T.);
#851=FACE_OUTER_BOUND('',#1035,.T.);
#852=FACE_OUTER_BOUND('',#1036,.T.);
#853=FACE_OUTER_BOUND('',#1037,.T.);
#854=FACE_OUTER_BOUND('',#1038,.T.);
#855=FACE_OUTER_BOUND('',#1039,.T.);
#856=FACE_OUTER_BOUND('',#1040,.T.);
#857=FACE_OUTER_BOUND('',#1041,.T.);
#858=FACE_OUTER_BOUND('',#1042,.T.);
#859=FACE_OUTER_BOUND('',#1043,.T.);
#860=FACE_OUTER_BOUND('',#1044,.T.);
#861=FACE_OUTER_BOUND('',#1045,.T.);
#862=FACE_OUTER_BOUND('',#1046,.T.);
#863=FACE_OUTER_BOUND('',#1047,.T.);
#864=FACE_OUTER_BOUND('',#1048,.T.);
#865=FACE_OUTER_BOUND('',#1049,.T.);
#866=FACE_OUTER_BOUND('',#1050,.T.);
#867=FACE_OUTER_BOUND('',#1051,.T.);
#868=FACE_OUTER_BOUND('',#1052,.T.);
#869=FACE_OUTER_BOUND('',#1053,.T.);
#870=FACE_OUTER_BOUND('',#1054,.T.);
#871=FACE_OUTER_BOUND('',#1055,.T.);
#872=FACE_OUTER_BOUND('',#1056,.T.);
#873=FACE_OUTER_BOUND('',#1057,.T.);
#874=FACE_OUTER_BOUND('',#1058,.T.);
#875=FACE_OUTER_BOUND('',#1059,.T.);
#876=FACE_OUTER_BOUND('',#1061,.T.);
#877=FACE_OUTER_BOUND('',#1062,.T.);
#878=FACE_OUTER_BOUND('',#1063,.T.);
#879=FACE_OUTER_BOUND('',#1064,.T.);
#880=FACE_OUTER_BOUND('',#1065,.T.);
#881=FACE_OUTER_BOUND('',#1066,.T.);
#882=FACE_OUTER_BOUND('',#1067,.T.);
#883=FACE_OUTER_BOUND('',#1068,.T.);
#884=FACE_OUTER_BOUND('',#1070,.T.);
#885=FACE_OUTER_BOUND('',#1071,.T.);
#886=FACE_OUTER_BOUND('',#1072,.T.);
#887=FACE_OUTER_BOUND('',#1073,.T.);
#888=FACE_OUTER_BOUND('',#1075,.T.);
#889=FACE_OUTER_BOUND('',#1076,.T.);
#890=FACE_OUTER_BOUND('',#1078,.T.);
#891=FACE_OUTER_BOUND('',#1080,.T.);
#892=FACE_OUTER_BOUND('',#1081,.T.);
#893=FACE_OUTER_BOUND('',#1082,.T.);
#894=FACE_OUTER_BOUND('',#1084,.T.);
#895=FACE_OUTER_BOUND('',#1085,.T.);
#896=FACE_OUTER_BOUND('',#1086,.T.);
#897=FACE_OUTER_BOUND('',#1087,.T.);
#898=FACE_OUTER_BOUND('',#1089,.T.);
#899=FACE_OUTER_BOUND('',#1090,.T.);
#900=FACE_OUTER_BOUND('',#1091,.T.);
#901=FACE_OUTER_BOUND('',#1092,.T.);
#902=FACE_OUTER_BOUND('',#1093,.T.);
#903=FACE_OUTER_BOUND('',#1094,.T.);
#904=FACE_OUTER_BOUND('',#1095,.T.);
#905=FACE_OUTER_BOUND('',#1096,.T.);
#906=FACE_OUTER_BOUND('',#1097,.T.);
#907=FACE_OUTER_BOUND('',#1098,.T.);
#908=FACE_OUTER_BOUND('',#1099,.T.);
#909=FACE_OUTER_BOUND('',#1101,.T.);
#910=EDGE_LOOP('',(#2080,#2081,#2082,#2083));
#911=EDGE_LOOP('',(#2084));
#912=EDGE_LOOP('',(#2085));
#913=EDGE_LOOP('',(#2086,#2087,#2088,#2089));
#914=EDGE_LOOP('',(#2090,#2091,#2092,#2093));
#915=EDGE_LOOP('',(#2094,#2095,#2096,#2097));
#916=EDGE_LOOP('',(#2098,#2099,#2100,#2101));
#917=EDGE_LOOP('',(#2102,#2103,#2104,#2105));
#918=EDGE_LOOP('',(#2106,#2107,#2108,#2109));
#919=EDGE_LOOP('',(#2110,#2111,#2112,#2113));
#920=EDGE_LOOP('',(#2114,#2115,#2116,#2117));
#921=EDGE_LOOP('',(#2118,#2119,#2120,#2121));
#922=EDGE_LOOP('',(#2122,#2123,#2124,#2125));
#923=EDGE_LOOP('',(#2126,#2127,#2128,#2129));
#924=EDGE_LOOP('',(#2130,#2131,#2132,#2133));
#925=EDGE_LOOP('',(#2134,#2135,#2136,#2137));
#926=EDGE_LOOP('',(#2138,#2139,#2140,#2141));
#927=EDGE_LOOP('',(#2142,#2143,#2144,#2145));
#928=EDGE_LOOP('',(#2146,#2147,#2148,#2149));
#929=EDGE_LOOP('',(#2150,#2151,#2152,#2153));
#930=EDGE_LOOP('',(#2154,#2155,#2156,#2157));
#931=EDGE_LOOP('',(#2158,#2159,#2160,#2161));
#932=EDGE_LOOP('',(#2162,#2163,#2164,#2165));
#933=EDGE_LOOP('',(#2166,#2167,#2168,#2169));
#934=EDGE_LOOP('',(#2170,#2171,#2172,#2173));
#935=EDGE_LOOP('',(#2174,#2175,#2176,#2177));
#936=EDGE_LOOP('',(#2178,#2179,#2180,#2181));
#937=EDGE_LOOP('',(#2182,#2183,#2184,#2185));
#938=EDGE_LOOP('',(#2186,#2187,#2188,#2189,#2190,#2191,#2192,#2193,#2194,
#2195,#2196,#2197,#2198,#2199,#2200,#2201,#2202,#2203,#2204,#2205,#2206,
#2207,#2208,#2209,#2210,#2211,#2212,#2213,#2214,#2215,#2216,#2217,#2218,
#2219,#2220,#2221,#2222,#2223,#2224,#2225,#2226,#2227,#2228,#2229,#2230,
#2231,#2232,#2233,#2234,#2235,#2236,#2237,#2238,#2239));
#939=EDGE_LOOP('',(#2240,#2241,#2242,#2243));
#940=EDGE_LOOP('',(#2244,#2245,#2246,#2247));
#941=EDGE_LOOP('',(#2248,#2249,#2250,#2251));
#942=EDGE_LOOP('',(#2252,#2253,#2254,#2255));
#943=EDGE_LOOP('',(#2256,#2257,#2258,#2259));
#944=EDGE_LOOP('',(#2260,#2261,#2262,#2263));
#945=EDGE_LOOP('',(#2264,#2265,#2266,#2267));
#946=EDGE_LOOP('',(#2268,#2269,#2270,#2271));
#947=EDGE_LOOP('',(#2272,#2273,#2274,#2275));
#948=EDGE_LOOP('',(#2276,#2277,#2278,#2279));
#949=EDGE_LOOP('',(#2280,#2281,#2282,#2283));
#950=EDGE_LOOP('',(#2284,#2285,#2286,#2287));
#951=EDGE_LOOP('',(#2288,#2289,#2290,#2291));
#952=EDGE_LOOP('',(#2292,#2293,#2294,#2295));
#953=EDGE_LOOP('',(#2296,#2297,#2298,#2299));
#954=EDGE_LOOP('',(#2300,#2301,#2302,#2303));
#955=EDGE_LOOP('',(#2304,#2305,#2306,#2307));
#956=EDGE_LOOP('',(#2308,#2309,#2310,#2311));
#957=EDGE_LOOP('',(#2312,#2313,#2314,#2315));
#958=EDGE_LOOP('',(#2316,#2317,#2318,#2319));
#959=EDGE_LOOP('',(#2320,#2321,#2322,#2323));
#960=EDGE_LOOP('',(#2324,#2325,#2326,#2327));
#961=EDGE_LOOP('',(#2328,#2329,#2330,#2331));
#962=EDGE_LOOP('',(#2332,#2333,#2334,#2335));
#963=EDGE_LOOP('',(#2336,#2337,#2338,#2339,#2340,#2341));
#964=EDGE_LOOP('',(#2342,#2343,#2344,#2345,#2346,#2347,#2348,#2349,#2350,
#2351,#2352,#2353,#2354,#2355,#2356,#2357,#2358,#2359,#2360,#2361,#2362,
#2363,#2364,#2365,#2366,#2367,#2368,#2369,#2370,#2371,#2372,#2373,#2374,
#2375,#2376,#2377,#2378,#2379,#2380,#2381,#2382,#2383,#2384,#2385,#2386,
#2387,#2388,#2389,#2390,#2391,#2392,#2393,#2394,#2395));
#965=EDGE_LOOP('',(#2396,#2397,#2398,#2399));
#966=EDGE_LOOP('',(#2400));
#967=EDGE_LOOP('',(#2401));
#968=EDGE_LOOP('',(#2402,#2403,#2404,#2405));
#969=EDGE_LOOP('',(#2406,#2407,#2408,#2409));
#970=EDGE_LOOP('',(#2410,#2411,#2412,#2413));
#971=EDGE_LOOP('',(#2414,#2415,#2416,#2417,#2418,#2419));
#972=EDGE_LOOP('',(#2420,#2421,#2422,#2423));
#973=EDGE_LOOP('',(#2424,#2425,#2426,#2427));
#974=EDGE_LOOP('',(#2428,#2429,#2430,#2431,#2432,#2433));
#975=EDGE_LOOP('',(#2434,#2435,#2436,#2437));
#976=EDGE_LOOP('',(#2438,#2439,#2440,#2441));
#977=EDGE_LOOP('',(#2442,#2443,#2444,#2445));
#978=EDGE_LOOP('',(#2446,#2447,#2448,#2449));
#979=EDGE_LOOP('',(#2450,#2451,#2452,#2453));
#980=EDGE_LOOP('',(#2454,#2455,#2456,#2457));
#981=EDGE_LOOP('',(#2458,#2459,#2460,#2461));
#982=EDGE_LOOP('',(#2462,#2463,#2464,#2465));
#983=EDGE_LOOP('',(#2466,#2467,#2468,#2469));
#984=EDGE_LOOP('',(#2470,#2471,#2472,#2473));
#985=EDGE_LOOP('',(#2474,#2475,#2476,#2477));
#986=EDGE_LOOP('',(#2478,#2479,#2480,#2481,#2482,#2483,#2484,#2485,#2486,
#2487,#2488,#2489,#2490,#2491,#2492,#2493,#2494,#2495,#2496,#2497));
#987=EDGE_LOOP('',(#2498));
#988=EDGE_LOOP('',(#2499,#2500,#2501,#2502));
#989=EDGE_LOOP('',(#2503,#2504,#2505,#2506));
#990=EDGE_LOOP('',(#2507,#2508,#2509,#2510));
#991=EDGE_LOOP('',(#2511,#2512,#2513,#2514));
#992=EDGE_LOOP('',(#2515,#2516,#2517,#2518));
#993=EDGE_LOOP('',(#2519,#2520,#2521,#2522));
#994=EDGE_LOOP('',(#2523,#2524,#2525,#2526));
#995=EDGE_LOOP('',(#2527,#2528,#2529,#2530));
#996=EDGE_LOOP('',(#2531,#2532,#2533,#2534));
#997=EDGE_LOOP('',(#2535,#2536,#2537,#2538,#2539,#2540,#2541,#2542,#2543,
#2544,#2545,#2546,#2547,#2548,#2549,#2550,#2551,#2552,#2553,#2554,#2555,
#2556,#2557,#2558));
#998=EDGE_LOOP('',(#2559,#2560,#2561,#2562,#2563));
#999=EDGE_LOOP('',(#2564,#2565,#2566,#2567));
#1000=EDGE_LOOP('',(#2568));
#1001=EDGE_LOOP('',(#2569,#2570,#2571,#2572));
#1002=EDGE_LOOP('',(#2573));
#1003=EDGE_LOOP('',(#2574,#2575,#2576,#2577));
#1004=EDGE_LOOP('',(#2578,#2579,#2580,#2581));
#1005=EDGE_LOOP('',(#2582,#2583,#2584,#2585));
#1006=EDGE_LOOP('',(#2586,#2587,#2588,#2589));
#1007=EDGE_LOOP('',(#2590,#2591,#2592,#2593));
#1008=EDGE_LOOP('',(#2594,#2595,#2596,#2597));
#1009=EDGE_LOOP('',(#2598,#2599,#2600,#2601));
#1010=EDGE_LOOP('',(#2602,#2603,#2604,#2605));
#1011=EDGE_LOOP('',(#2606,#2607,#2608,#2609));
#1012=EDGE_LOOP('',(#2610,#2611,#2612,#2613));
#1013=EDGE_LOOP('',(#2614,#2615,#2616,#2617));
#1014=EDGE_LOOP('',(#2618,#2619,#2620,#2621));
#1015=EDGE_LOOP('',(#2622,#2623,#2624,#2625));
#1016=EDGE_LOOP('',(#2626,#2627,#2628,#2629));
#1017=EDGE_LOOP('',(#2630,#2631,#2632,#2633));
#1018=EDGE_LOOP('',(#2634,#2635,#2636,#2637));
#1019=EDGE_LOOP('',(#2638,#2639,#2640,#2641));
#1020=EDGE_LOOP('',(#2642,#2643,#2644,#2645));
#1021=EDGE_LOOP('',(#2646,#2647,#2648,#2649));
#1022=EDGE_LOOP('',(#2650,#2651,#2652,#2653));
#1023=EDGE_LOOP('',(#2654,#2655,#2656,#2657));
#1024=EDGE_LOOP('',(#2658,#2659,#2660,#2661));
#1025=EDGE_LOOP('',(#2662,#2663,#2664,#2665));
#1026=EDGE_LOOP('',(#2666,#2667,#2668,#2669));
#1027=EDGE_LOOP('',(#2670,#2671,#2672,#2673,#2674,#2675,#2676,#2677,#2678,
#2679,#2680,#2681,#2682,#2683,#2684,#2685,#2686,#2687,#2688,#2689,#2690,
#2691,#2692,#2693,#2694,#2695,#2696,#2697,#2698,#2699,#2700,#2701,#2702,
#2703,#2704,#2705,#2706,#2707,#2708,#2709,#2710,#2711,#2712,#2713,#2714,
#2715,#2716,#2717,#2718,#2719,#2720,#2721,#2722,#2723));
#1028=EDGE_LOOP('',(#2724,#2725,#2726,#2727));
#1029=EDGE_LOOP('',(#2728,#2729,#2730,#2731));
#1030=EDGE_LOOP('',(#2732,#2733,#2734,#2735));
#1031=EDGE_LOOP('',(#2736,#2737,#2738,#2739));
#1032=EDGE_LOOP('',(#2740,#2741,#2742,#2743));
#1033=EDGE_LOOP('',(#2744,#2745,#2746,#2747));
#1034=EDGE_LOOP('',(#2748,#2749,#2750,#2751));
#1035=EDGE_LOOP('',(#2752,#2753,#2754,#2755));
#1036=EDGE_LOOP('',(#2756,#2757,#2758,#2759));
#1037=EDGE_LOOP('',(#2760,#2761,#2762,#2763));
#1038=EDGE_LOOP('',(#2764,#2765,#2766,#2767));
#1039=EDGE_LOOP('',(#2768,#2769,#2770,#2771));
#1040=EDGE_LOOP('',(#2772,#2773,#2774,#2775));
#1041=EDGE_LOOP('',(#2776,#2777,#2778,#2779));
#1042=EDGE_LOOP('',(#2780,#2781,#2782,#2783));
#1043=EDGE_LOOP('',(#2784,#2785,#2786,#2787));
#1044=EDGE_LOOP('',(#2788,#2789,#2790,#2791));
#1045=EDGE_LOOP('',(#2792,#2793,#2794,#2795));
#1046=EDGE_LOOP('',(#2796,#2797,#2798,#2799));
#1047=EDGE_LOOP('',(#2800,#2801,#2802,#2803));
#1048=EDGE_LOOP('',(#2804,#2805,#2806,#2807));
#1049=EDGE_LOOP('',(#2808,#2809,#2810,#2811));
#1050=EDGE_LOOP('',(#2812,#2813,#2814,#2815));
#1051=EDGE_LOOP('',(#2816,#2817,#2818,#2819));
#1052=EDGE_LOOP('',(#2820,#2821,#2822,#2823,#2824,#2825));
#1053=EDGE_LOOP('',(#2826,#2827,#2828,#2829));
#1054=EDGE_LOOP('',(#2830));
#1055=EDGE_LOOP('',(#2831));
#1056=EDGE_LOOP('',(#2832,#2833,#2834,#2835));
#1057=EDGE_LOOP('',(#2836,#2837,#2838,#2839,#2840,#2841,#2842,#2843,#2844,
#2845,#2846,#2847,#2848,#2849,#2850,#2851,#2852,#2853,#2854,#2855,#2856,
#2857,#2858,#2859,#2860,#2861,#2862,#2863,#2864,#2865,#2866,#2867,#2868,
#2869,#2870,#2871,#2872,#2873,#2874,#2875,#2876,#2877,#2878,#2879,#2880,
#2881,#2882,#2883,#2884,#2885,#2886,#2887,#2888,#2889));
#1058=EDGE_LOOP('',(#2890,#2891,#2892,#2893));
#1059=EDGE_LOOP('',(#2894,#2895,#2896,#2897,#2898,#2899));
#1060=EDGE_LOOP('',(#2900,#2901,#2902,#2903));
#1061=EDGE_LOOP('',(#2904,#2905,#2906,#2907));
#1062=EDGE_LOOP('',(#2908,#2909,#2910,#2911,#2912));
#1063=EDGE_LOOP('',(#2913,#2914,#2915,#2916,#2917,#2918));
#1064=EDGE_LOOP('',(#2919));
#1065=EDGE_LOOP('',(#2920,#2921,#2922,#2923));
#1066=EDGE_LOOP('',(#2924,#2925,#2926,#2927,#2928));
#1067=EDGE_LOOP('',(#2929,#2930,#2931,#2932,#2933));
#1068=EDGE_LOOP('',(#2934));
#1069=EDGE_LOOP('',(#2935));
#1070=EDGE_LOOP('',(#2936,#2937,#2938,#2939,#2940));
#1071=EDGE_LOOP('',(#2941,#2942,#2943,#2944));
#1072=EDGE_LOOP('',(#2945,#2946,#2947,#2948,#2949,#2950,#2951,#2952,#2953,
#2954,#2955,#2956,#2957,#2958,#2959,#2960,#2961));
#1073=EDGE_LOOP('',(#2962));
#1074=EDGE_LOOP('',(#2963,#2964));
#1075=EDGE_LOOP('',(#2965,#2966,#2967,#2968));
#1076=EDGE_LOOP('',(#2969));
#1077=EDGE_LOOP('',(#2970));
#1078=EDGE_LOOP('',(#2971,#2972));
#1079=EDGE_LOOP('',(#2973));
#1080=EDGE_LOOP('',(#2974,#2975,#2976,#2977));
#1081=EDGE_LOOP('',(#2978,#2979,#2980,#2981,#2982,#2983));
#1082=EDGE_LOOP('',(#2984));
#1083=EDGE_LOOP('',(#2985,#2986));
#1084=EDGE_LOOP('',(#2987));
#1085=EDGE_LOOP('',(#2988,#2989,#2990,#2991));
#1086=EDGE_LOOP('',(#2992,#2993,#2994,#2995));
#1087=EDGE_LOOP('',(#2996));
#1088=EDGE_LOOP('',(#2997));
#1089=EDGE_LOOP('',(#2998,#2999,#3000,#3001));
#1090=EDGE_LOOP('',(#3002));
#1091=EDGE_LOOP('',(#3003,#3004,#3005,#3006));
#1092=EDGE_LOOP('',(#3007));
#1093=EDGE_LOOP('',(#3008,#3009));
#1094=EDGE_LOOP('',(#3010,#3011,#3012,#3013));
#1095=EDGE_LOOP('',(#3014));
#1096=EDGE_LOOP('',(#3015));
#1097=EDGE_LOOP('',(#3016,#3017,#3018,#3019));
#1098=EDGE_LOOP('',(#3020,#3021,#3022,#3023));
#1099=EDGE_LOOP('',(#3024));
#1100=EDGE_LOOP('',(#3025));
#1101=EDGE_LOOP('',(#3026));
#1102=EDGE_LOOP('',(#3027));
#1103=CIRCLE('',#3338,10.5057959473896);
#1104=CIRCLE('',#3339,0.5);
#1105=CIRCLE('',#3340,10.0057959473896);
#1106=CIRCLE('',#3342,9.50579594738959);
#1107=CIRCLE('',#3344,10.5057959473896);
#1108=CIRCLE('',#3370,10.5246348408465);
#1109=CIRCLE('',#3371,11.0246348408465);
#1110=CIRCLE('',#3372,11.0246348408465);
#1111=CIRCLE('',#3373,11.0246348408465);
#1112=CIRCLE('',#3374,11.0246348408465);
#1113=CIRCLE('',#3375,11.0246348408465);
#1114=CIRCLE('',#3376,11.0246348408465);
#1115=CIRCLE('',#3377,11.0246348408465);
#1116=CIRCLE('',#3378,11.0246348408465);
#1117=CIRCLE('',#3379,11.0246348408465);
#1118=CIRCLE('',#3380,11.0246348408465);
#1119=CIRCLE('',#3381,11.0246348408465);
#1120=CIRCLE('',#3382,11.0246348408465);
#1121=CIRCLE('',#3383,11.0246348408465);
#1122=CIRCLE('',#3384,11.0246348408465);
#1123=CIRCLE('',#3385,11.0246348408465);
#1124=CIRCLE('',#3386,11.0246348408465);
#1125=CIRCLE('',#3387,11.0246348408465);
#1126=CIRCLE('',#3388,11.0246348408465);
#1127=CIRCLE('',#3389,11.0246348408465);
#1128=CIRCLE('',#3390,11.0246348408465);
#1129=CIRCLE('',#3391,11.0246348408465);
#1130=CIRCLE('',#3392,11.0246348408465);
#1131=CIRCLE('',#3393,11.0246348408465);
#1132=CIRCLE('',#3394,11.0246348408465);
#1133=CIRCLE('',#3395,11.0246348408465);
#1134=CIRCLE('',#3397,11.0246348408465);
#1135=CIRCLE('',#3399,11.0246348408465);
#1136=CIRCLE('',#3401,11.0246348408465);
#1137=CIRCLE('',#3403,11.0246348408465);
#1138=CIRCLE('',#3405,11.0246348408465);
#1139=CIRCLE('',#3407,11.0246348408465);
#1140=CIRCLE('',#3409,11.0246348408465);
#1141=CIRCLE('',#3411,11.0246348408465);
#1142=CIRCLE('',#3413,11.0246348408465);
#1143=CIRCLE('',#3415,11.0246348408465);
#1144=CIRCLE('',#3417,11.0246348408465);
#1145=CIRCLE('',#3419,11.0246348408465);
#1146=CIRCLE('',#3421,11.0246348408465);
#1147=CIRCLE('',#3423,11.0246348408465);
#1148=CIRCLE('',#3425,11.0246348408465);
#1149=CIRCLE('',#3427,11.0246348408465);
#1150=CIRCLE('',#3429,11.0246348408465);
#1151=CIRCLE('',#3431,11.0246348408465);
#1152=CIRCLE('',#3433,11.0246348408465);
#1153=CIRCLE('',#3435,11.0246348408465);
#1154=CIRCLE('',#3437,11.0246348408465);
#1155=CIRCLE('',#3439,11.0246348408465);
#1156=CIRCLE('',#3441,11.0246348408465);
#1157=CIRCLE('',#3443,11.0246348408465);
#1158=CIRCLE('',#3446,11.0246348408465);
#1159=CIRCLE('',#3450,9.50579594738959);
#1160=CIRCLE('',#3454,5.72286361298787);
#1161=CIRCLE('',#3455,6.22286361298787);
#1162=CIRCLE('',#3457,4.72286361298787);
#1163=CIRCLE('',#3460,5.72286361298787);
#1164=CIRCLE('',#3461,6.22286361298787);
#1165=CIRCLE('',#3465,4.72286361298787);
#1166=CIRCLE('',#3469,0.5);
#1167=CIRCLE('',#3471,0.5);
#1168=CIRCLE('',#3473,0.5);
#1169=CIRCLE('',#3475,0.5);
#1170=CIRCLE('',#3477,0.5);
#1171=CIRCLE('',#3479,0.5);
#1172=CIRCLE('',#3481,0.5);
#1173=CIRCLE('',#3483,0.5);
#1174=CIRCLE('',#3485,0.5);
#1175=CIRCLE('',#3487,2.);
#1176=CIRCLE('',#3488,2.);
#1177=CIRCLE('',#3489,2.);
#1178=CIRCLE('',#3490,2.);
#1179=CIRCLE('',#3491,2.);
#1180=CIRCLE('',#3492,2.);
#1181=CIRCLE('',#3493,2.);
#1182=CIRCLE('',#3494,2.);
#1183=CIRCLE('',#3495,2.);
#1184=CIRCLE('',#3496,0.5);
#1185=CIRCLE('',#3497,2.);
#1186=CIRCLE('',#3498,1.);
#1187=CIRCLE('',#3500,2.);
#1188=CIRCLE('',#3502,2.);
#1189=CIRCLE('',#3504,2.);
#1190=CIRCLE('',#3506,2.);
#1191=CIRCLE('',#3508,2.);
#1192=CIRCLE('',#3510,2.);
#1193=CIRCLE('',#3512,2.);
#1194=CIRCLE('',#3514,2.);
#1195=CIRCLE('',#3516,2.);
#1196=CIRCLE('',#3518,1.5);
#1197=CIRCLE('',#3519,0.5);
#1198=CIRCLE('',#3520,2.);
#1199=CIRCLE('',#3525,1.);
#1200=CIRCLE('',#3553,9.50579594738959);
#1201=CIRCLE('',#3554,11.0246348408465);
#1202=CIRCLE('',#3555,11.0246348408465);
#1203=CIRCLE('',#3556,11.0246348408465);
#1204=CIRCLE('',#3557,11.0246348408465);
#1205=CIRCLE('',#3558,11.0246348408465);
#1206=CIRCLE('',#3559,11.0246348408465);
#1207=CIRCLE('',#3560,11.0246348408465);
#1208=CIRCLE('',#3561,11.0246348408465);
#1209=CIRCLE('',#3562,11.0246348408465);
#1210=CIRCLE('',#3563,11.0246348408465);
#1211=CIRCLE('',#3564,11.0246348408465);
#1212=CIRCLE('',#3565,11.0246348408465);
#1213=CIRCLE('',#3566,11.0246348408465);
#1214=CIRCLE('',#3567,11.0246348408465);
#1215=CIRCLE('',#3568,11.0246348408465);
#1216=CIRCLE('',#3569,11.0246348408465);
#1217=CIRCLE('',#3570,11.0246348408465);
#1218=CIRCLE('',#3571,11.0246348408465);
#1219=CIRCLE('',#3572,11.0246348408465);
#1220=CIRCLE('',#3573,11.0246348408465);
#1221=CIRCLE('',#3574,11.0246348408465);
#1222=CIRCLE('',#3575,11.0246348408465);
#1223=CIRCLE('',#3576,11.0246348408465);
#1224=CIRCLE('',#3577,11.0246348408465);
#1225=CIRCLE('',#3578,11.0246348408465);
#1226=CIRCLE('',#3580,11.0246348408465);
#1227=CIRCLE('',#3582,11.0246348408465);
#1228=CIRCLE('',#3584,11.0246348408465);
#1229=CIRCLE('',#3586,11.0246348408465);
#1230=CIRCLE('',#3588,11.0246348408465);
#1231=CIRCLE('',#3590,11.0246348408465);
#1232=CIRCLE('',#3592,11.0246348408465);
#1233=CIRCLE('',#3594,11.0246348408465);
#1234=CIRCLE('',#3596,11.0246348408465);
#1235=CIRCLE('',#3598,11.0246348408465);
#1236=CIRCLE('',#3600,11.0246348408465);
#1237=CIRCLE('',#3602,11.0246348408465);
#1238=CIRCLE('',#3604,11.0246348408465);
#1239=CIRCLE('',#3606,11.0246348408465);
#1240=CIRCLE('',#3608,11.0246348408465);
#1241=CIRCLE('',#3610,11.0246348408465);
#1242=CIRCLE('',#3612,11.0246348408465);
#1243=CIRCLE('',#3614,11.0246348408465);
#1244=CIRCLE('',#3616,11.0246348408465);
#1245=CIRCLE('',#3618,11.0246348408465);
#1246=CIRCLE('',#3620,11.0246348408465);
#1247=CIRCLE('',#3622,11.0246348408465);
#1248=CIRCLE('',#3624,11.0246348408465);
#1249=CIRCLE('',#3626,11.0246348408465);
#1250=CIRCLE('',#3629,9.50579594738959);
#1251=CIRCLE('',#3632,9.50579594738959);
#1252=CIRCLE('',#3634,9.50579594738959);
#1253=CIRCLE('',#3636,11.0246348408465);
#1254=CIRCLE('',#3640,9.50563484084649);
#1255=CIRCLE('',#3641,9.50563484084649);
#1256=CIRCLE('',#3642,9.50563484084649);
#1257=CIRCLE('',#3643,9.50563484084649);
#1258=CIRCLE('',#3647,1.);
#1259=CIRCLE('',#3652,4.72286361298787);
#1260=CIRCLE('',#3653,4.72286361298787);
#1261=CIRCLE('',#3654,4.22286361298787);
#1262=CIRCLE('',#3656,3.72286361298787);
#1263=CIRCLE('',#3658,4.72286361298787);
#1264=CIRCLE('',#3660,10.5246348408465);
#1265=CIRCLE('',#3661,0.5);
#1266=CIRCLE('',#3662,11.0246348408465);
#1267=CIRCLE('',#3664,11.0246348408465);
#1268=CIRCLE('',#3667,0.5);
#1269=CIRCLE('',#3668,10.5246348408465);
#1270=CIRCLE('',#3671,3.72286361298787);
#1271=CIRCLE('',#3675,1.48244108211373);
#1272=CIRCLE('',#3676,1.5);
#1273=CIRCLE('',#3677,1.48244108211373);
#1274=CIRCLE('',#3678,1.5);
#1275=CIRCLE('',#3680,1.51706056234455);
#1276=CIRCLE('',#3682,1.51706056234455);
#1277=CIRCLE('',#3686,3.22286361298787);
#1278=CIRCLE('',#3687,3.72286361298787);
#1279=CIRCLE('',#3689,1.51706056234455);
#1280=CIRCLE('',#3691,3.72286361298787);
#1281=CIRCLE('',#3693,1.51706056234455);
#1282=CIRCLE('',#3698,1.5);
#1283=CIRCLE('',#3701,2.);
#1284=CIRCLE('',#3702,2.);
#1285=CIRCLE('',#3707,3.72286361298787);
#1286=CIRCLE('',#3708,3.72286361298787);
#1287=CIRCLE('',#3710,5.22286361298787);
#1288=CIRCLE('',#3711,5.22286361298787);
#1289=VERTEX_POINT('',#4665);
#1290=VERTEX_POINT('',#4667);
#1291=VERTEX_POINT('',#4671);
#1292=VERTEX_POINT('',#4674);
#1293=VERTEX_POINT('',#4678);
#1294=VERTEX_POINT('',#4679);
#1295=VERTEX_POINT('',#4694);
#1296=VERTEX_POINT('',#4696);
#1297=VERTEX_POINT('',#4713);
#1298=VERTEX_POINT('',#4714);
#1299=VERTEX_POINT('',#4729);
#1300=VERTEX_POINT('',#4731);
#1301=VERTEX_POINT('',#4748);
#1302=VERTEX_POINT('',#4749);
#1303=VERTEX_POINT('',#4764);
#1304=VERTEX_POINT('',#4766);
#1305=VERTEX_POINT('',#4783);
#1306=VERTEX_POINT('',#4784);
#1307=VERTEX_POINT('',#4799);
#1308=VERTEX_POINT('',#4801);
#1309=VERTEX_POINT('',#4818);
#1310=VERTEX_POINT('',#4819);
#1311=VERTEX_POINT('',#4834);
#1312=VERTEX_POINT('',#4836);
#1313=VERTEX_POINT('',#4853);
#1314=VERTEX_POINT('',#4854);
#1315=VERTEX_POINT('',#4869);
#1316=VERTEX_POINT('',#4871);
#1317=VERTEX_POINT('',#4888);
#1318=VERTEX_POINT('',#4889);
#1319=VERTEX_POINT('',#4904);
#1320=VERTEX_POINT('',#4906);
#1321=VERTEX_POINT('',#4923);
#1322=VERTEX_POINT('',#4924);
#1323=VERTEX_POINT('',#4939);
#1324=VERTEX_POINT('',#4941);
#1325=VERTEX_POINT('',#4958);
#1326=VERTEX_POINT('',#4959);
#1327=VERTEX_POINT('',#4974);
#1328=VERTEX_POINT('',#4976);
#1329=VERTEX_POINT('',#4993);
#1330=VERTEX_POINT('',#4994);
#1331=VERTEX_POINT('',#5009);
#1332=VERTEX_POINT('',#5011);
#1333=VERTEX_POINT('',#5028);
#1334=VERTEX_POINT('',#5029);
#1335=VERTEX_POINT('',#5044);
#1336=VERTEX_POINT('',#5046);
#1337=VERTEX_POINT('',#5063);
#1338=VERTEX_POINT('',#5064);
#1339=VERTEX_POINT('',#5079);
#1340=VERTEX_POINT('',#5081);
#1341=VERTEX_POINT('',#5098);
#1342=VERTEX_POINT('',#5099);
#1343=VERTEX_POINT('',#5114);
#1344=VERTEX_POINT('',#5116);
#1345=VERTEX_POINT('',#5133);
#1346=VERTEX_POINT('',#5134);
#1347=VERTEX_POINT('',#5149);
#1348=VERTEX_POINT('',#5151);
#1349=VERTEX_POINT('',#5168);
#1350=VERTEX_POINT('',#5169);
#1351=VERTEX_POINT('',#5184);
#1352=VERTEX_POINT('',#5186);
#1353=VERTEX_POINT('',#5203);
#1354=VERTEX_POINT('',#5204);
#1355=VERTEX_POINT('',#5219);
#1356=VERTEX_POINT('',#5221);
#1357=VERTEX_POINT('',#5238);
#1358=VERTEX_POINT('',#5239);
#1359=VERTEX_POINT('',#5254);
#1360=VERTEX_POINT('',#5256);
#1361=VERTEX_POINT('',#5273);
#1362=VERTEX_POINT('',#5274);
#1363=VERTEX_POINT('',#5289);
#1364=VERTEX_POINT('',#5291);
#1365=VERTEX_POINT('',#5308);
#1366=VERTEX_POINT('',#5309);
#1367=VERTEX_POINT('',#5324);
#1368=VERTEX_POINT('',#5326);
#1369=VERTEX_POINT('',#5343);
#1370=VERTEX_POINT('',#5344);
#1371=VERTEX_POINT('',#5359);
#1372=VERTEX_POINT('',#5361);
#1373=VERTEX_POINT('',#5378);
#1374=VERTEX_POINT('',#5379);
#1375=VERTEX_POINT('',#5394);
#1376=VERTEX_POINT('',#5396);
#1377=VERTEX_POINT('',#5413);
#1378=VERTEX_POINT('',#5414);
#1379=VERTEX_POINT('',#5429);
#1380=VERTEX_POINT('',#5431);
#1381=VERTEX_POINT('',#5448);
#1382=VERTEX_POINT('',#5449);
#1383=VERTEX_POINT('',#5464);
#1384=VERTEX_POINT('',#5466);
#1385=VERTEX_POINT('',#5483);
#1386=VERTEX_POINT('',#5484);
#1387=VERTEX_POINT('',#5499);
#1388=VERTEX_POINT('',#5501);
#1389=VERTEX_POINT('',#5518);
#1390=VERTEX_POINT('',#5520);
#1391=VERTEX_POINT('',#5522);
#1392=VERTEX_POINT('',#5555);
#1393=VERTEX_POINT('',#5566);
#1394=VERTEX_POINT('',#5570);
#1395=VERTEX_POINT('',#5618);
#1396=VERTEX_POINT('',#5641);
#1397=VERTEX_POINT('',#5647);
#1398=VERTEX_POINT('',#5648);
#1399=VERTEX_POINT('',#5652);
#1400=VERTEX_POINT('',#5654);
#1401=VERTEX_POINT('',#5660);
#1402=VERTEX_POINT('',#5662);
#1403=VERTEX_POINT('',#5666);
#1404=VERTEX_POINT('',#5668);
#1405=VERTEX_POINT('',#5672);
#1406=VERTEX_POINT('',#5676);
#1407=VERTEX_POINT('',#5677);
#1408=VERTEX_POINT('',#5686);
#1409=VERTEX_POINT('',#5694);
#1410=VERTEX_POINT('',#5695);
#1411=VERTEX_POINT('',#5697);
#1412=VERTEX_POINT('',#5720);
#1413=VERTEX_POINT('',#5724);
#1414=VERTEX_POINT('',#5725);
#1415=VERTEX_POINT('',#5727);
#1416=VERTEX_POINT('',#5750);
#1417=VERTEX_POINT('',#5754);
#1418=VERTEX_POINT('',#5755);
#1419=VERTEX_POINT('',#5757);
#1420=VERTEX_POINT('',#5780);
#1421=VERTEX_POINT('',#5784);
#1422=VERTEX_POINT('',#5785);
#1423=VERTEX_POINT('',#5787);
#1424=VERTEX_POINT('',#5810);
#1425=VERTEX_POINT('',#5814);
#1426=VERTEX_POINT('',#5815);
#1427=VERTEX_POINT('',#5817);
#1428=VERTEX_POINT('',#5844);
#1429=VERTEX_POINT('',#5848);
#1430=VERTEX_POINT('',#5849);
#1431=VERTEX_POINT('',#5851);
#1432=VERTEX_POINT('',#5874);
#1433=VERTEX_POINT('',#5878);
#1434=VERTEX_POINT('',#5879);
#1435=VERTEX_POINT('',#5881);
#1436=VERTEX_POINT('',#5904);
#1437=VERTEX_POINT('',#5908);
#1438=VERTEX_POINT('',#5909);
#1439=VERTEX_POINT('',#5911);
#1440=VERTEX_POINT('',#5934);
#1441=VERTEX_POINT('',#5938);
#1442=VERTEX_POINT('',#5939);
#1443=VERTEX_POINT('',#5941);
#1444=VERTEX_POINT('',#5964);
#1445=VERTEX_POINT('',#5976);
#1446=VERTEX_POINT('',#5978);
#1447=VERTEX_POINT('',#5981);
#1448=VERTEX_POINT('',#5984);
#1449=VERTEX_POINT('',#6004);
#1450=VERTEX_POINT('',#6006);
#1451=VERTEX_POINT('',#6020);
#1452=VERTEX_POINT('',#6043);
#1453=VERTEX_POINT('',#6049);
#1454=VERTEX_POINT('',#6050);
#1455=VERTEX_POINT('',#6065);
#1456=VERTEX_POINT('',#6067);
#1457=VERTEX_POINT('',#6084);
#1458=VERTEX_POINT('',#6085);
#1459=VERTEX_POINT('',#6100);
#1460=VERTEX_POINT('',#6102);
#1461=VERTEX_POINT('',#6119);
#1462=VERTEX_POINT('',#6120);
#1463=VERTEX_POINT('',#6135);
#1464=VERTEX_POINT('',#6137);
#1465=VERTEX_POINT('',#6154);
#1466=VERTEX_POINT('',#6155);
#1467=VERTEX_POINT('',#6170);
#1468=VERTEX_POINT('',#6172);
#1469=VERTEX_POINT('',#6189);
#1470=VERTEX_POINT('',#6190);
#1471=VERTEX_POINT('',#6205);
#1472=VERTEX_POINT('',#6207);
#1473=VERTEX_POINT('',#6224);
#1474=VERTEX_POINT('',#6225);
#1475=VERTEX_POINT('',#6240);
#1476=VERTEX_POINT('',#6242);
#1477=VERTEX_POINT('',#6259);
#1478=VERTEX_POINT('',#6260);
#1479=VERTEX_POINT('',#6275);
#1480=VERTEX_POINT('',#6277);
#1481=VERTEX_POINT('',#6294);
#1482=VERTEX_POINT('',#6295);
#1483=VERTEX_POINT('',#6310);
#1484=VERTEX_POINT('',#6312);
#1485=VERTEX_POINT('',#6329);
#1486=VERTEX_POINT('',#6330);
#1487=VERTEX_POINT('',#6345);
#1488=VERTEX_POINT('',#6347);
#1489=VERTEX_POINT('',#6364);
#1490=VERTEX_POINT('',#6365);
#1491=VERTEX_POINT('',#6380);
#1492=VERTEX_POINT('',#6382);
#1493=VERTEX_POINT('',#6399);
#1494=VERTEX_POINT('',#6400);
#1495=VERTEX_POINT('',#6415);
#1496=VERTEX_POINT('',#6417);
#1497=VERTEX_POINT('',#6434);
#1498=VERTEX_POINT('',#6435);
#1499=VERTEX_POINT('',#6450);
#1500=VERTEX_POINT('',#6452);
#1501=VERTEX_POINT('',#6469);
#1502=VERTEX_POINT('',#6470);
#1503=VERTEX_POINT('',#6485);
#1504=VERTEX_POINT('',#6487);
#1505=VERTEX_POINT('',#6504);
#1506=VERTEX_POINT('',#6505);
#1507=VERTEX_POINT('',#6520);
#1508=VERTEX_POINT('',#6522);
#1509=VERTEX_POINT('',#6539);
#1510=VERTEX_POINT('',#6540);
#1511=VERTEX_POINT('',#6555);
#1512=VERTEX_POINT('',#6557);
#1513=VERTEX_POINT('',#6574);
#1514=VERTEX_POINT('',#6575);
#1515=VERTEX_POINT('',#6590);
#1516=VERTEX_POINT('',#6592);
#1517=VERTEX_POINT('',#6609);
#1518=VERTEX_POINT('',#6610);
#1519=VERTEX_POINT('',#6625);
#1520=VERTEX_POINT('',#6627);
#1521=VERTEX_POINT('',#6644);
#1522=VERTEX_POINT('',#6645);
#1523=VERTEX_POINT('',#6660);
#1524=VERTEX_POINT('',#6662);
#1525=VERTEX_POINT('',#6679);
#1526=VERTEX_POINT('',#6680);
#1527=VERTEX_POINT('',#6695);
#1528=VERTEX_POINT('',#6697);
#1529=VERTEX_POINT('',#6714);
#1530=VERTEX_POINT('',#6715);
#1531=VERTEX_POINT('',#6730);
#1532=VERTEX_POINT('',#6732);
#1533=VERTEX_POINT('',#6749);
#1534=VERTEX_POINT('',#6750);
#1535=VERTEX_POINT('',#6765);
#1536=VERTEX_POINT('',#6767);
#1537=VERTEX_POINT('',#6784);
#1538=VERTEX_POINT('',#6785);
#1539=VERTEX_POINT('',#6800);
#1540=VERTEX_POINT('',#6802);
#1541=VERTEX_POINT('',#6819);
#1542=VERTEX_POINT('',#6820);
#1543=VERTEX_POINT('',#6835);
#1544=VERTEX_POINT('',#6837);
#1545=VERTEX_POINT('',#6854);
#1546=VERTEX_POINT('',#6855);
#1547=VERTEX_POINT('',#6870);
#1548=VERTEX_POINT('',#6872);
#1549=VERTEX_POINT('',#6889);
#1550=VERTEX_POINT('',#6891);
#1551=VERTEX_POINT('',#6893);
#1552=VERTEX_POINT('',#6926);
#1553=VERTEX_POINT('',#6937);
#1554=VERTEX_POINT('',#6941);
#1555=VERTEX_POINT('',#6989);
#1556=VERTEX_POINT('',#7007);
#1557=VERTEX_POINT('',#7012);
#1558=VERTEX_POINT('',#7015);
#1559=VERTEX_POINT('',#7024);
#1560=VERTEX_POINT('',#7025);
#1561=VERTEX_POINT('',#7028);
#1562=VERTEX_POINT('',#7030);
#1563=VERTEX_POINT('',#7033);
#1564=VERTEX_POINT('',#7034);
#1565=VERTEX_POINT('',#7036);
#1566=VERTEX_POINT('',#7055);
#1567=VERTEX_POINT('',#7076);
#1568=VERTEX_POINT('',#7078);
#1569=VERTEX_POINT('',#7082);
#1570=VERTEX_POINT('',#7084);
#1571=VERTEX_POINT('',#7106);
#1572=VERTEX_POINT('',#7107);
#1573=VERTEX_POINT('',#7118);
#1574=VERTEX_POINT('',#7129);
#1575=VERTEX_POINT('',#7152);
#1576=VERTEX_POINT('',#7156);
#1577=VERTEX_POINT('',#7178);
#1578=VERTEX_POINT('',#7179);
#1579=VERTEX_POINT('',#7182);
#1580=VERTEX_POINT('',#7186);
#1581=VERTEX_POINT('',#7189);
#1582=VERTEX_POINT('',#7193);
#1583=VERTEX_POINT('',#7195);
#1584=VERTEX_POINT('',#7201);
#1585=VERTEX_POINT('',#7206);
#1586=VERTEX_POINT('',#7211);
#1587=VERTEX_POINT('',#7217);
#1588=VERTEX_POINT('',#7218);
#1589=VERTEX_POINT('',#7220);
#1590=VERTEX_POINT('',#7223);
#1591=VERTEX_POINT('',#7226);
#1592=VERTEX_POINT('',#7229);
#1593=VERTEX_POINT('',#7235);
#1594=VERTEX_POINT('',#7237);
#1595=VERTEX_POINT('',#7241);
#1596=VERTEX_POINT('',#7244);
#1597=VERTEX_POINT('',#7248);
#1598=VERTEX_POINT('',#7255);
#1599=VERTEX_POINT('',#7256);
#1600=VERTEX_POINT('',#7260);
#1601=VERTEX_POINT('',#7262);
#1602=VERTEX_POINT('',#7269);
#1603=VERTEX_POINT('',#7271);
#1604=VERTEX_POINT('',#7275);
#1605=VERTEX_POINT('',#7277);
#1606=EDGE_CURVE('',#1289,#1289,#1103,.T.);
#1607=EDGE_CURVE('',#1289,#1290,#1104,.T.);
#1608=EDGE_CURVE('',#1290,#1290,#1105,.T.);
#1609=EDGE_CURVE('',#1291,#1291,#1106,.T.);
#1610=EDGE_CURVE('',#1292,#1292,#1107,.T.);
#1611=EDGE_CURVE('',#1292,#1289,#229,.T.);
#1612=EDGE_CURVE('',#1293,#1294,#105,.T.);
#1613=EDGE_CURVE('',#1295,#1293,#230,.T.);
#1614=EDGE_CURVE('',#1296,#1295,#106,.T.);
#1615=EDGE_CURVE('',#1294,#1296,#231,.T.);
#1616=EDGE_CURVE('',#1297,#1298,#107,.T.);
#1617=EDGE_CURVE('',#1299,#1297,#232,.T.);
#1618=EDGE_CURVE('',#1300,#1299,#108,.T.);
#1619=EDGE_CURVE('',#1298,#1300,#233,.T.);
#1620=EDGE_CURVE('',#1301,#1302,#109,.T.);
#1621=EDGE_CURVE('',#1303,#1301,#234,.T.);
#1622=EDGE_CURVE('',#1304,#1303,#110,.T.);
#1623=EDGE_CURVE('',#1302,#1304,#235,.T.);
#1624=EDGE_CURVE('',#1305,#1306,#111,.T.);
#1625=EDGE_CURVE('',#1307,#1305,#236,.T.);
#1626=EDGE_CURVE('',#1308,#1307,#112,.T.);
#1627=EDGE_CURVE('',#1306,#1308,#237,.T.);
#1628=EDGE_CURVE('',#1309,#1310,#113,.T.);
#1629=EDGE_CURVE('',#1311,#1309,#238,.T.);
#1630=EDGE_CURVE('',#1312,#1311,#114,.T.);
#1631=EDGE_CURVE('',#1310,#1312,#239,.T.);
#1632=EDGE_CURVE('',#1313,#1314,#115,.T.);
#1633=EDGE_CURVE('',#1315,#1313,#240,.T.);
#1634=EDGE_CURVE('',#1316,#1315,#116,.T.);
#1635=EDGE_CURVE('',#1314,#1316,#241,.T.);
#1636=EDGE_CURVE('',#1317,#1318,#117,.T.);
#1637=EDGE_CURVE('',#1319,#1317,#242,.T.);
#1638=EDGE_CURVE('',#1320,#1319,#118,.T.);
#1639=EDGE_CURVE('',#1318,#1320,#243,.T.);
#1640=EDGE_CURVE('',#1321,#1322,#119,.T.);
#1641=EDGE_CURVE('',#1323,#1321,#244,.T.);
#1642=EDGE_CURVE('',#1324,#1323,#120,.T.);
#1643=EDGE_CURVE('',#1322,#1324,#245,.T.);
#1644=EDGE_CURVE('',#1325,#1326,#121,.T.);
#1645=EDGE_CURVE('',#1327,#1325,#246,.T.);
#1646=EDGE_CURVE('',#1328,#1327,#122,.T.);
#1647=EDGE_CURVE('',#1326,#1328,#247,.T.);
#1648=EDGE_CURVE('',#1329,#1330,#123,.T.);
#1649=EDGE_CURVE('',#1331,#1329,#248,.T.);
#1650=EDGE_CURVE('',#1332,#1331,#124,.T.);
#1651=EDGE_CURVE('',#1330,#1332,#249,.T.);
#1652=EDGE_CURVE('',#1333,#1334,#125,.T.);
#1653=EDGE_CURVE('',#1335,#1333,#250,.T.);
#1654=EDGE_CURVE('',#1336,#1335,#126,.T.);
#1655=EDGE_CURVE('',#1334,#1336,#251,.T.);
#1656=EDGE_CURVE('',#1337,#1338,#127,.T.);
#1657=EDGE_CURVE('',#1339,#1337,#252,.T.);
#1658=EDGE_CURVE('',#1340,#1339,#128,.T.);
#1659=EDGE_CURVE('',#1338,#1340,#253,.T.);
#1660=EDGE_CURVE('',#1341,#1342,#129,.T.);
#1661=EDGE_CURVE('',#1343,#1341,#254,.T.);
#1662=EDGE_CURVE('',#1344,#1343,#130,.T.);
#1663=EDGE_CURVE('',#1342,#1344,#255,.T.);
#1664=EDGE_CURVE('',#1345,#1346,#131,.T.);
#1665=EDGE_CURVE('',#1347,#1345,#256,.T.);
#1666=EDGE_CURVE('',#1348,#1347,#132,.T.);
#1667=EDGE_CURVE('',#1346,#1348,#257,.T.);
#1668=EDGE_CURVE('',#1349,#1350,#133,.T.);
#1669=EDGE_CURVE('',#1351,#1349,#258,.T.);
#1670=EDGE_CURVE('',#1352,#1351,#134,.T.);
#1671=EDGE_CURVE('',#1350,#1352,#259,.T.);
#1672=EDGE_CURVE('',#1353,#1354,#135,.T.);
#1673=EDGE_CURVE('',#1355,#1353,#260,.T.);
#1674=EDGE_CURVE('',#1356,#1355,#136,.T.);
#1675=EDGE_CURVE('',#1354,#1356,#261,.T.);
#1676=EDGE_CURVE('',#1357,#1358,#137,.T.);
#1677=EDGE_CURVE('',#1359,#1357,#262,.T.);
#1678=EDGE_CURVE('',#1360,#1359,#138,.T.);
#1679=EDGE_CURVE('',#1358,#1360,#263,.T.);
#1680=EDGE_CURVE('',#1361,#1362,#139,.T.);
#1681=EDGE_CURVE('',#1363,#1361,#264,.T.);
#1682=EDGE_CURVE('',#1364,#1363,#140,.T.);
#1683=EDGE_CURVE('',#1362,#1364,#265,.T.);
#1684=EDGE_CURVE('',#1365,#1366,#141,.T.);
#1685=EDGE_CURVE('',#1367,#1365,#266,.T.);
#1686=EDGE_CURVE('',#1368,#1367,#142,.T.);
#1687=EDGE_CURVE('',#1366,#1368,#267,.T.);
#1688=EDGE_CURVE('',#1369,#1370,#143,.T.);
#1689=EDGE_CURVE('',#1371,#1369,#268,.T.);
#1690=EDGE_CURVE('',#1372,#1371,#144,.T.);
#1691=EDGE_CURVE('',#1370,#1372,#269,.T.);
#1692=EDGE_CURVE('',#1373,#1374,#145,.T.);
#1693=EDGE_CURVE('',#1375,#1373,#270,.T.);
#1694=EDGE_CURVE('',#1376,#1375,#146,.T.);
#1695=EDGE_CURVE('',#1374,#1376,#271,.T.);
#1696=EDGE_CURVE('',#1377,#1378,#147,.T.);
#1697=EDGE_CURVE('',#1379,#1377,#272,.T.);
#1698=EDGE_CURVE('',#1380,#1379,#148,.T.);
#1699=EDGE_CURVE('',#1378,#1380,#273,.T.);
#1700=EDGE_CURVE('',#1381,#1382,#149,.T.);
#1701=EDGE_CURVE('',#1383,#1381,#274,.T.);
#1702=EDGE_CURVE('',#1384,#1383,#150,.T.);
#1703=EDGE_CURVE('',#1382,#1384,#275,.T.);
#1704=EDGE_CURVE('',#1385,#1386,#151,.T.);
#1705=EDGE_CURVE('',#1387,#1385,#276,.T.);
#1706=EDGE_CURVE('',#1388,#1387,#152,.T.);
#1707=EDGE_CURVE('',#1386,#1388,#277,.T.);
#1708=EDGE_CURVE('',#1389,#1389,#1108,.T.);
#1709=EDGE_CURVE('',#1389,#1390,#278,.T.);
#1710=EDGE_CURVE('',#1390,#1391,#153,.T.);
#1711=EDGE_CURVE('',#1391,#1388,#1109,.T.);
#1712=EDGE_CURVE('',#1387,#1384,#1110,.T.);
#1713=EDGE_CURVE('',#1383,#1380,#1111,.T.);
#1714=EDGE_CURVE('',#1379,#1376,#1112,.T.);
#1715=EDGE_CURVE('',#1375,#1372,#1113,.T.);
#1716=EDGE_CURVE('',#1371,#1368,#1114,.T.);
#1717=EDGE_CURVE('',#1367,#1364,#1115,.T.);
#1718=EDGE_CURVE('',#1363,#1360,#1116,.T.);
#1719=EDGE_CURVE('',#1359,#1356,#1117,.T.);
#1720=EDGE_CURVE('',#1355,#1352,#1118,.T.);
#1721=EDGE_CURVE('',#1351,#1348,#1119,.T.);
#1722=EDGE_CURVE('',#1347,#1344,#1120,.T.);
#1723=EDGE_CURVE('',#1343,#1340,#1121,.T.);
#1724=EDGE_CURVE('',#1339,#1336,#1122,.T.);
#1725=EDGE_CURVE('',#1335,#1332,#1123,.T.);
#1726=EDGE_CURVE('',#1331,#1328,#1124,.T.);
#1727=EDGE_CURVE('',#1327,#1324,#1125,.T.);
#1728=EDGE_CURVE('',#1323,#1320,#1126,.T.);
#1729=EDGE_CURVE('',#1319,#1316,#1127,.T.);
#1730=EDGE_CURVE('',#1315,#1312,#1128,.T.);
#1731=EDGE_CURVE('',#1311,#1308,#1129,.T.);
#1732=EDGE_CURVE('',#1307,#1304,#1130,.T.);
#1733=EDGE_CURVE('',#1303,#1300,#1131,.T.);
#1734=EDGE_CURVE('',#1299,#1296,#1132,.T.);
#1735=EDGE_CURVE('',#1295,#1392,#1133,.T.);
#1736=EDGE_CURVE('',#1392,#1390,#154,.T.);
#1737=EDGE_CURVE('',#1293,#1393,#1134,.T.);
#1738=EDGE_CURVE('',#1393,#1392,#279,.T.);
#1739=EDGE_CURVE('',#1391,#1394,#280,.T.);
#1740=EDGE_CURVE('',#1394,#1386,#1135,.T.);
#1741=EDGE_CURVE('',#1385,#1382,#1136,.T.);
#1742=EDGE_CURVE('',#1381,#1378,#1137,.T.);
#1743=EDGE_CURVE('',#1377,#1374,#1138,.T.);
#1744=EDGE_CURVE('',#1373,#1370,#1139,.T.);
#1745=EDGE_CURVE('',#1369,#1366,#1140,.T.);
#1746=EDGE_CURVE('',#1365,#1362,#1141,.T.);
#1747=EDGE_CURVE('',#1361,#1358,#1142,.T.);
#1748=EDGE_CURVE('',#1357,#1354,#1143,.T.);
#1749=EDGE_CURVE('',#1353,#1350,#1144,.T.);
#1750=EDGE_CURVE('',#1349,#1346,#1145,.T.);
#1751=EDGE_CURVE('',#1345,#1342,#1146,.T.);
#1752=EDGE_CURVE('',#1341,#1338,#1147,.T.);
#1753=EDGE_CURVE('',#1337,#1334,#1148,.T.);
#1754=EDGE_CURVE('',#1333,#1330,#1149,.T.);
#1755=EDGE_CURVE('',#1329,#1326,#1150,.T.);
#1756=EDGE_CURVE('',#1325,#1322,#1151,.T.);
#1757=EDGE_CURVE('',#1321,#1318,#1152,.T.);
#1758=EDGE_CURVE('',#1317,#1314,#1153,.T.);
#1759=EDGE_CURVE('',#1313,#1310,#1154,.T.);
#1760=EDGE_CURVE('',#1309,#1306,#1155,.T.);
#1761=EDGE_CURVE('',#1305,#1302,#1156,.T.);
#1762=EDGE_CURVE('',#1301,#1298,#1157,.T.);
#1763=EDGE_CURVE('',#1394,#1395,#155,.T.);
#1764=EDGE_CURVE('',#1395,#1393,#156,.T.);
#1765=EDGE_CURVE('',#1297,#1294,#1158,.T.);
#1766=EDGE_CURVE('',#1395,#1292,#281,.T.);
#1767=EDGE_CURVE('',#1396,#1396,#1159,.T.);
#1768=EDGE_CURVE('',#1396,#1291,#282,.T.);
#1769=EDGE_CURVE('',#1397,#1398,#53,.T.);
#1770=EDGE_CURVE('',#1398,#1399,#1160,.T.);
#1771=EDGE_CURVE('',#1399,#1400,#54,.T.);
#1772=EDGE_CURVE('',#1400,#1397,#1161,.T.);
#1773=EDGE_CURVE('',#1398,#1401,#283,.T.);
#1774=EDGE_CURVE('',#1401,#1402,#1162,.T.);
#1775=EDGE_CURVE('',#1402,#1399,#284,.T.);
#1776=EDGE_CURVE('',#1403,#1397,#285,.T.);
#1777=EDGE_CURVE('',#1404,#1403,#55,.T.);
#1778=EDGE_CURVE('',#1404,#1405,#286,.T.);
#1779=EDGE_CURVE('',#1405,#1401,#287,.T.);
#1780=EDGE_CURVE('',#1406,#1407,#56,.T.);
#1781=EDGE_CURVE('',#1407,#1404,#1163,.T.);
#1782=EDGE_CURVE('',#1403,#1406,#1164,.T.);
#1783=EDGE_CURVE('',#1406,#1400,#288,.F.);
#1784=EDGE_CURVE('',#1408,#1402,#289,.T.);
#1785=EDGE_CURVE('',#1408,#1407,#290,.T.);
#1786=EDGE_CURVE('',#1405,#1408,#1165,.T.);
#1787=EDGE_CURVE('',#1409,#1410,#291,.T.);
#1788=EDGE_CURVE('',#1411,#1409,#157,.T.);
#1789=EDGE_CURVE('',#1412,#1411,#292,.T.);
#1790=EDGE_CURVE('',#1410,#1412,#1166,.T.);
#1791=EDGE_CURVE('',#1413,#1414,#293,.T.);
#1792=EDGE_CURVE('',#1415,#1413,#158,.T.);
#1793=EDGE_CURVE('',#1416,#1415,#294,.T.);
#1794=EDGE_CURVE('',#1414,#1416,#1167,.T.);
#1795=EDGE_CURVE('',#1417,#1418,#295,.T.);
#1796=EDGE_CURVE('',#1419,#1417,#159,.T.);
#1797=EDGE_CURVE('',#1420,#1419,#296,.T.);
#1798=EDGE_CURVE('',#1418,#1420,#1168,.T.);
#1799=EDGE_CURVE('',#1421,#1422,#297,.T.);
#1800=EDGE_CURVE('',#1423,#1421,#160,.T.);
#1801=EDGE_CURVE('',#1424,#1423,#298,.T.);
#1802=EDGE_CURVE('',#1422,#1424,#1169,.T.);
#1803=EDGE_CURVE('',#1425,#1426,#299,.T.);
#1804=EDGE_CURVE('',#1427,#1425,#161,.T.);
#1805=EDGE_CURVE('',#1428,#1427,#300,.T.);
#1806=EDGE_CURVE('',#1426,#1428,#1170,.T.);
#1807=EDGE_CURVE('',#1429,#1430,#301,.T.);
#1808=EDGE_CURVE('',#1431,#1429,#162,.T.);
#1809=EDGE_CURVE('',#1432,#1431,#302,.T.);
#1810=EDGE_CURVE('',#1430,#1432,#1171,.T.);
#1811=EDGE_CURVE('',#1433,#1434,#303,.T.);
#1812=EDGE_CURVE('',#1435,#1433,#163,.T.);
#1813=EDGE_CURVE('',#1436,#1435,#304,.T.);
#1814=EDGE_CURVE('',#1434,#1436,#1172,.T.);
#1815=EDGE_CURVE('',#1437,#1438,#305,.T.);
#1816=EDGE_CURVE('',#1439,#1437,#164,.T.);
#1817=EDGE_CURVE('',#1440,#1439,#306,.T.);
#1818=EDGE_CURVE('',#1438,#1440,#1173,.T.);
#1819=EDGE_CURVE('',#1441,#1442,#307,.T.);
#1820=EDGE_CURVE('',#1443,#1441,#165,.T.);
#1821=EDGE_CURVE('',#1444,#1443,#308,.T.);
#1822=EDGE_CURVE('',#1442,#1444,#1174,.T.);
#1823=EDGE_CURVE('',#1414,#1412,#1175,.T.);
#1824=EDGE_CURVE('',#1418,#1416,#1176,.T.);
#1825=EDGE_CURVE('',#1422,#1420,#1177,.T.);
#1826=EDGE_CURVE('',#1426,#1424,#1178,.T.);
#1827=EDGE_CURVE('',#1430,#1428,#1179,.T.);
#1828=EDGE_CURVE('',#1434,#1432,#1180,.T.);
#1829=EDGE_CURVE('',#1438,#1436,#1181,.T.);
#1830=EDGE_CURVE('',#1442,#1440,#1182,.T.);
#1831=EDGE_CURVE('',#1445,#1444,#1183,.T.);
#1832=EDGE_CURVE('',#1445,#1446,#1184,.T.);
#1833=EDGE_CURVE('',#1410,#1446,#1185,.T.);
#1834=EDGE_CURVE('',#1447,#1447,#1186,.T.);
#1835=EDGE_CURVE('',#1448,#1443,#1187,.T.);
#1836=EDGE_CURVE('',#1448,#1445,#309,.T.);
#1837=EDGE_CURVE('',#1441,#1439,#1188,.T.);
#1838=EDGE_CURVE('',#1437,#1435,#1189,.T.);
#1839=EDGE_CURVE('',#1433,#1431,#1190,.T.);
#1840=EDGE_CURVE('',#1429,#1427,#1191,.T.);
#1841=EDGE_CURVE('',#1425,#1423,#1192,.T.);
#1842=EDGE_CURVE('',#1421,#1419,#1193,.T.);
#1843=EDGE_CURVE('',#1417,#1415,#1194,.T.);
#1844=EDGE_CURVE('',#1413,#1411,#1195,.T.);
#1845=EDGE_CURVE('',#1449,#1449,#1196,.T.);
#1846=EDGE_CURVE('',#1449,#1450,#1197,.T.);
#1847=EDGE_CURVE('',#1450,#1448,#166,.T.);
#1848=EDGE_CURVE('',#1409,#1451,#1198,.T.);
#1849=EDGE_CURVE('',#1451,#1450,#167,.T.);
#1850=EDGE_CURVE('',#1446,#1451,#310,.T.);
#1851=EDGE_CURVE('',#1452,#1452,#1199,.T.);
#1852=EDGE_CURVE('',#1452,#1447,#311,.T.);
#1853=EDGE_CURVE('',#1453,#1454,#168,.T.);
#1854=EDGE_CURVE('',#1455,#1453,#312,.T.);
#1855=EDGE_CURVE('',#1456,#1455,#169,.T.);
#1856=EDGE_CURVE('',#1454,#1456,#313,.T.);
#1857=EDGE_CURVE('',#1457,#1458,#170,.T.);
#1858=EDGE_CURVE('',#1459,#1457,#314,.T.);
#1859=EDGE_CURVE('',#1460,#1459,#171,.T.);
#1860=EDGE_CURVE('',#1458,#1460,#315,.T.);
#1861=EDGE_CURVE('',#1461,#1462,#172,.T.);
#1862=EDGE_CURVE('',#1463,#1461,#316,.T.);
#1863=EDGE_CURVE('',#1464,#1463,#173,.T.);
#1864=EDGE_CURVE('',#1462,#1464,#317,.T.);
#1865=EDGE_CURVE('',#1465,#1466,#174,.T.);
#1866=EDGE_CURVE('',#1467,#1465,#318,.T.);
#1867=EDGE_CURVE('',#1468,#1467,#175,.T.);
#1868=EDGE_CURVE('',#1466,#1468,#319,.T.);
#1869=EDGE_CURVE('',#1469,#1470,#176,.T.);
#1870=EDGE_CURVE('',#1471,#1469,#320,.T.);
#1871=EDGE_CURVE('',#1472,#1471,#177,.T.);
#1872=EDGE_CURVE('',#1470,#1472,#321,.T.);
#1873=EDGE_CURVE('',#1473,#1474,#178,.T.);
#1874=EDGE_CURVE('',#1475,#1473,#322,.T.);
#1875=EDGE_CURVE('',#1476,#1475,#179,.T.);
#1876=EDGE_CURVE('',#1474,#1476,#323,.T.);
#1877=EDGE_CURVE('',#1477,#1478,#180,.T.);
#1878=EDGE_CURVE('',#1479,#1477,#324,.T.);
#1879=EDGE_CURVE('',#1480,#1479,#181,.T.);
#1880=EDGE_CURVE('',#1478,#1480,#325,.T.);
#1881=EDGE_CURVE('',#1481,#1482,#182,.T.);
#1882=EDGE_CURVE('',#1483,#1481,#326,.T.);
#1883=EDGE_CURVE('',#1484,#1483,#183,.T.);
#1884=EDGE_CURVE('',#1482,#1484,#327,.T.);
#1885=EDGE_CURVE('',#1485,#1486,#184,.T.);
#1886=EDGE_CURVE('',#1487,#1485,#328,.T.);
#1887=EDGE_CURVE('',#1488,#1487,#185,.T.);
#1888=EDGE_CURVE('',#1486,#1488,#329,.T.);
#1889=EDGE_CURVE('',#1489,#1490,#186,.T.);
#1890=EDGE_CURVE('',#1491,#1489,#330,.T.);
#1891=EDGE_CURVE('',#1492,#1491,#187,.T.);
#1892=EDGE_CURVE('',#1490,#1492,#331,.T.);
#1893=EDGE_CURVE('',#1493,#1494,#188,.T.);
#1894=EDGE_CURVE('',#1495,#1493,#332,.T.);
#1895=EDGE_CURVE('',#1496,#1495,#189,.T.);
#1896=EDGE_CURVE('',#1494,#1496,#333,.T.);
#1897=EDGE_CURVE('',#1497,#1498,#190,.T.);
#1898=EDGE_CURVE('',#1499,#1497,#334,.T.);
#1899=EDGE_CURVE('',#1500,#1499,#191,.T.);
#1900=EDGE_CURVE('',#1498,#1500,#335,.T.);
#1901=EDGE_CURVE('',#1501,#1502,#192,.T.);
#1902=EDGE_CURVE('',#1503,#1501,#336,.T.);
#1903=EDGE_CURVE('',#1504,#1503,#193,.T.);
#1904=EDGE_CURVE('',#1502,#1504,#337,.T.);
#1905=EDGE_CURVE('',#1505,#1506,#194,.T.);
#1906=EDGE_CURVE('',#1507,#1505,#338,.T.);
#1907=EDGE_CURVE('',#1508,#1507,#195,.T.);
#1908=EDGE_CURVE('',#1506,#1508,#339,.T.);
#1909=EDGE_CURVE('',#1509,#1510,#196,.T.);
#1910=EDGE_CURVE('',#1511,#1509,#340,.T.);
#1911=EDGE_CURVE('',#1512,#1511,#197,.T.);
#1912=EDGE_CURVE('',#1510,#1512,#341,.T.);
#1913=EDGE_CURVE('',#1513,#1514,#198,.T.);
#1914=EDGE_CURVE('',#1515,#1513,#342,.T.);
#1915=EDGE_CURVE('',#1516,#1515,#199,.T.);
#1916=EDGE_CURVE('',#1514,#1516,#343,.T.);
#1917=EDGE_CURVE('',#1517,#1518,#200,.T.);
#1918=EDGE_CURVE('',#1519,#1517,#344,.T.);
#1919=EDGE_CURVE('',#1520,#1519,#201,.T.);
#1920=EDGE_CURVE('',#1518,#1520,#345,.T.);
#1921=EDGE_CURVE('',#1521,#1522,#202,.T.);
#1922=EDGE_CURVE('',#1523,#1521,#346,.T.);
#1923=EDGE_CURVE('',#1524,#1523,#203,.T.);
#1924=EDGE_CURVE('',#1522,#1524,#347,.T.);
#1925=EDGE_CURVE('',#1525,#1526,#204,.T.);
#1926=EDGE_CURVE('',#1527,#1525,#348,.T.);
#1927=EDGE_CURVE('',#1528,#1527,#205,.T.);
#1928=EDGE_CURVE('',#1526,#1528,#349,.T.);
#1929=EDGE_CURVE('',#1529,#1530,#206,.T.);
#1930=EDGE_CURVE('',#1531,#1529,#350,.T.);
#1931=EDGE_CURVE('',#1532,#1531,#207,.T.);
#1932=EDGE_CURVE('',#1530,#1532,#351,.T.);
#1933=EDGE_CURVE('',#1533,#1534,#208,.T.);
#1934=EDGE_CURVE('',#1535,#1533,#352,.T.);
#1935=EDGE_CURVE('',#1536,#1535,#209,.T.);
#1936=EDGE_CURVE('',#1534,#1536,#353,.T.);
#1937=EDGE_CURVE('',#1537,#1538,#210,.T.);
#1938=EDGE_CURVE('',#1539,#1537,#354,.T.);
#1939=EDGE_CURVE('',#1540,#1539,#211,.T.);
#1940=EDGE_CURVE('',#1538,#1540,#355,.T.);
#1941=EDGE_CURVE('',#1541,#1542,#212,.T.);
#1942=EDGE_CURVE('',#1543,#1541,#356,.T.);
#1943=EDGE_CURVE('',#1544,#1543,#213,.T.);
#1944=EDGE_CURVE('',#1542,#1544,#357,.T.);
#1945=EDGE_CURVE('',#1545,#1546,#214,.T.);
#1946=EDGE_CURVE('',#1547,#1545,#358,.T.);
#1947=EDGE_CURVE('',#1548,#1547,#215,.T.);
#1948=EDGE_CURVE('',#1546,#1548,#359,.T.);
#1949=EDGE_CURVE('',#1549,#1549,#1200,.T.);
#1950=EDGE_CURVE('',#1549,#1550,#360,.T.);
#1951=EDGE_CURVE('',#1550,#1551,#216,.T.);
#1952=EDGE_CURVE('',#1551,#1548,#1201,.T.);
#1953=EDGE_CURVE('',#1547,#1544,#1202,.T.);
#1954=EDGE_CURVE('',#1543,#1540,#1203,.T.);
#1955=EDGE_CURVE('',#1539,#1536,#1204,.T.);
#1956=EDGE_CURVE('',#1535,#1532,#1205,.T.);
#1957=EDGE_CURVE('',#1531,#1528,#1206,.T.);
#1958=EDGE_CURVE('',#1527,#1524,#1207,.T.);
#1959=EDGE_CURVE('',#1523,#1520,#1208,.T.);
#1960=EDGE_CURVE('',#1519,#1516,#1209,.T.);
#1961=EDGE_CURVE('',#1515,#1512,#1210,.T.);
#1962=EDGE_CURVE('',#1511,#1508,#1211,.T.);
#1963=EDGE_CURVE('',#1507,#1504,#1212,.T.);
#1964=EDGE_CURVE('',#1503,#1500,#1213,.T.);
#1965=EDGE_CURVE('',#1499,#1496,#1214,.T.);
#1966=EDGE_CURVE('',#1495,#1492,#1215,.T.);
#1967=EDGE_CURVE('',#1491,#1488,#1216,.T.);
#1968=EDGE_CURVE('',#1487,#1484,#1217,.T.);
#1969=EDGE_CURVE('',#1483,#1480,#1218,.T.);
#1970=EDGE_CURVE('',#1479,#1476,#1219,.T.);
#1971=EDGE_CURVE('',#1475,#1472,#1220,.T.);
#1972=EDGE_CURVE('',#1471,#1468,#1221,.T.);
#1973=EDGE_CURVE('',#1467,#1464,#1222,.T.);
#1974=EDGE_CURVE('',#1463,#1460,#1223,.T.);
#1975=EDGE_CURVE('',#1459,#1456,#1224,.T.);
#1976=EDGE_CURVE('',#1455,#1552,#1225,.T.);
#1977=EDGE_CURVE('',#1552,#1550,#217,.T.);
#1978=EDGE_CURVE('',#1453,#1553,#1226,.T.);
#1979=EDGE_CURVE('',#1553,#1552,#361,.T.);
#1980=EDGE_CURVE('',#1551,#1554,#362,.T.);
#1981=EDGE_CURVE('',#1554,#1546,#1227,.T.);
#1982=EDGE_CURVE('',#1545,#1542,#1228,.T.);
#1983=EDGE_CURVE('',#1541,#1538,#1229,.T.);
#1984=EDGE_CURVE('',#1537,#1534,#1230,.T.);
#1985=EDGE_CURVE('',#1533,#1530,#1231,.T.);
#1986=EDGE_CURVE('',#1529,#1526,#1232,.T.);
#1987=EDGE_CURVE('',#1525,#1522,#1233,.T.);
#1988=EDGE_CURVE('',#1521,#1518,#1234,.T.);
#1989=EDGE_CURVE('',#1517,#1514,#1235,.T.);
#1990=EDGE_CURVE('',#1513,#1510,#1236,.T.);
#1991=EDGE_CURVE('',#1509,#1506,#1237,.T.);
#1992=EDGE_CURVE('',#1505,#1502,#1238,.T.);
#1993=EDGE_CURVE('',#1501,#1498,#1239,.T.);
#1994=EDGE_CURVE('',#1497,#1494,#1240,.T.);
#1995=EDGE_CURVE('',#1493,#1490,#1241,.T.);
#1996=EDGE_CURVE('',#1489,#1486,#1242,.T.);
#1997=EDGE_CURVE('',#1485,#1482,#1243,.T.);
#1998=EDGE_CURVE('',#1481,#1478,#1244,.T.);
#1999=EDGE_CURVE('',#1477,#1474,#1245,.T.);
#2000=EDGE_CURVE('',#1473,#1470,#1246,.T.);
#2001=EDGE_CURVE('',#1469,#1466,#1247,.T.);
#2002=EDGE_CURVE('',#1465,#1462,#1248,.T.);
#2003=EDGE_CURVE('',#1461,#1458,#1249,.T.);
#2004=EDGE_CURVE('',#1554,#1555,#218,.T.);
#2005=EDGE_CURVE('',#1555,#1553,#219,.T.);
#2006=EDGE_CURVE('',#1556,#1556,#1250,.T.);
#2007=EDGE_CURVE('',#1556,#1549,#363,.T.);
#2008=EDGE_CURVE('',#1557,#1557,#1251,.T.);
#2009=EDGE_CURVE('',#1558,#1558,#1252,.T.);
#2010=EDGE_CURVE('',#1558,#1557,#364,.T.);
#2011=EDGE_CURVE('',#1457,#1454,#1253,.T.);
#2012=EDGE_CURVE('',#1555,#1558,#365,.T.);
#2013=EDGE_CURVE('',#1559,#1560,#1254,.T.);
#2014=EDGE_CURVE('',#1560,#1559,#1255,.T.);
#2015=EDGE_CURVE('',#1559,#1561,#366,.T.);
#2016=EDGE_CURVE('',#1562,#1561,#1256,.T.);
#2017=EDGE_CURVE('',#1561,#1562,#1257,.T.);
#2018=EDGE_CURVE('',#1563,#1564,#367,.T.);
#2019=EDGE_CURVE('',#1565,#1563,#220,.T.);
#2020=EDGE_CURVE('',#1566,#1565,#368,.T.);
#2021=EDGE_CURVE('',#1564,#1566,#221,.T.);
#2022=EDGE_CURVE('',#1565,#1567,#369,.T.);
#2023=EDGE_CURVE('',#1568,#1567,#370,.T.);
#2024=EDGE_CURVE('',#1566,#1568,#371,.T.);
#2025=EDGE_CURVE('',#1563,#1569,#372,.T.);
#2026=EDGE_CURVE('',#1570,#1569,#222,.T.);
#2027=EDGE_CURVE('',#1567,#1570,#223,.T.);
#2028=EDGE_CURVE('',#1571,#1572,#224,.T.);
#2029=EDGE_CURVE('',#1573,#1571,#225,.T.);
#2030=EDGE_CURVE('',#1573,#1574,#373,.T.);
#2031=EDGE_CURVE('',#1574,#1574,#1258,.T.);
#2032=EDGE_CURVE('',#1572,#1573,#226,.T.);
#2033=EDGE_CURVE('',#1564,#1575,#374,.T.);
#2034=EDGE_CURVE('',#1569,#1575,#375,.T.);
#2035=EDGE_CURVE('',#1576,#1568,#227,.T.);
#2036=EDGE_CURVE('',#1575,#1576,#228,.T.);
#2037=EDGE_CURVE('',#1577,#1578,#1259,.T.);
#2038=EDGE_CURVE('',#1578,#1577,#1260,.T.);
#2039=EDGE_CURVE('',#1577,#1579,#376,.T.);
#2040=EDGE_CURVE('',#1579,#1579,#1261,.T.);
#2041=EDGE_CURVE('',#1580,#1580,#1262,.T.);
#2042=EDGE_CURVE('',#1581,#1581,#1263,.T.);
#2043=EDGE_CURVE('',#1581,#1578,#377,.T.);
#2044=EDGE_CURVE('',#1582,#1582,#1264,.T.);
#2045=EDGE_CURVE('',#1582,#1583,#1265,.T.);
#2046=EDGE_CURVE('',#1583,#1583,#1266,.T.);
#2047=EDGE_CURVE('',#1583,#1570,#378,.T.);
#2048=EDGE_CURVE('',#1576,#1572,#379,.T.);
#2049=EDGE_CURVE('',#1573,#1584,#380,.T.);
#2050=EDGE_CURVE('',#1584,#1584,#1267,.T.);
#2051=EDGE_CURVE('',#1584,#1585,#1268,.T.);
#2052=EDGE_CURVE('',#1585,#1585,#1269,.T.);
#2053=EDGE_CURVE('',#1586,#1586,#1270,.T.);
#2054=EDGE_CURVE('',#1586,#1580,#381,.T.);
#2055=EDGE_CURVE('',#1587,#1588,#1271,.T.);
#2056=EDGE_CURVE('',#1587,#1589,#1272,.T.);
#2057=EDGE_CURVE('',#1588,#1587,#1273,.T.);
#2058=EDGE_CURVE('',#1590,#1588,#1274,.T.);
#2059=EDGE_CURVE('',#1591,#1591,#1275,.T.);
#2060=EDGE_CURVE('',#1592,#1592,#1276,.T.);
#2061=EDGE_CURVE('',#1592,#1591,#382,.T.);
#2062=EDGE_CURVE('',#1593,#1593,#1277,.T.);
#2063=EDGE_CURVE('',#1593,#1594,#383,.T.);
#2064=EDGE_CURVE('',#1594,#1594,#1278,.T.);
#2065=EDGE_CURVE('',#1595,#1595,#1279,.T.);
#2066=EDGE_CURVE('',#1596,#1596,#1280,.T.);
#2067=EDGE_CURVE('',#1596,#1594,#384,.T.);
#2068=EDGE_CURVE('',#1597,#1597,#1281,.T.);
#2069=EDGE_CURVE('',#1595,#1597,#385,.T.);
#2070=EDGE_CURVE('',#1598,#1599,#1282,.T.);
#2071=EDGE_CURVE('',#1600,#1600,#1283,.T.);
#2072=EDGE_CURVE('',#1600,#1601,#386,.T.);
#2073=EDGE_CURVE('',#1601,#1601,#1284,.T.);
#2074=EDGE_CURVE('',#1602,#1602,#1285,.T.);
#2075=EDGE_CURVE('',#1602,#1603,#387,.T.);
#2076=EDGE_CURVE('',#1603,#1603,#1286,.T.);
#2077=EDGE_CURVE('',#1604,#1604,#1287,.T.);
#2078=EDGE_CURVE('',#1604,#1605,#388,.T.);
#2079=EDGE_CURVE('',#1605,#1605,#1288,.T.);
#2080=ORIENTED_EDGE('',*,*,#1606,.T.);
#2081=ORIENTED_EDGE('',*,*,#1607,.T.);
#2082=ORIENTED_EDGE('',*,*,#1608,.T.);
#2083=ORIENTED_EDGE('',*,*,#1607,.F.);
#2084=ORIENTED_EDGE('',*,*,#1608,.F.);
#2085=ORIENTED_EDGE('',*,*,#1609,.T.);
#2086=ORIENTED_EDGE('',*,*,#1610,.F.);
#2087=ORIENTED_EDGE('',*,*,#1611,.T.);
#2088=ORIENTED_EDGE('',*,*,#1606,.F.);
#2089=ORIENTED_EDGE('',*,*,#1611,.F.);
#2090=ORIENTED_EDGE('',*,*,#1612,.F.);
#2091=ORIENTED_EDGE('',*,*,#1613,.F.);
#2092=ORIENTED_EDGE('',*,*,#1614,.F.);
#2093=ORIENTED_EDGE('',*,*,#1615,.F.);
#2094=ORIENTED_EDGE('',*,*,#1616,.F.);
#2095=ORIENTED_EDGE('',*,*,#1617,.F.);
#2096=ORIENTED_EDGE('',*,*,#1618,.F.);
#2097=ORIENTED_EDGE('',*,*,#1619,.F.);
#2098=ORIENTED_EDGE('',*,*,#1620,.F.);
#2099=ORIENTED_EDGE('',*,*,#1621,.F.);
#2100=ORIENTED_EDGE('',*,*,#1622,.F.);
#2101=ORIENTED_EDGE('',*,*,#1623,.F.);
#2102=ORIENTED_EDGE('',*,*,#1624,.F.);
#2103=ORIENTED_EDGE('',*,*,#1625,.F.);
#2104=ORIENTED_EDGE('',*,*,#1626,.F.);
#2105=ORIENTED_EDGE('',*,*,#1627,.F.);
#2106=ORIENTED_EDGE('',*,*,#1628,.F.);
#2107=ORIENTED_EDGE('',*,*,#1629,.F.);
#2108=ORIENTED_EDGE('',*,*,#1630,.F.);
#2109=ORIENTED_EDGE('',*,*,#1631,.F.);
#2110=ORIENTED_EDGE('',*,*,#1632,.F.);
#2111=ORIENTED_EDGE('',*,*,#1633,.F.);
#2112=ORIENTED_EDGE('',*,*,#1634,.F.);
#2113=ORIENTED_EDGE('',*,*,#1635,.F.);
#2114=ORIENTED_EDGE('',*,*,#1636,.F.);
#2115=ORIENTED_EDGE('',*,*,#1637,.F.);
#2116=ORIENTED_EDGE('',*,*,#1638,.F.);
#2117=ORIENTED_EDGE('',*,*,#1639,.F.);
#2118=ORIENTED_EDGE('',*,*,#1640,.F.);
#2119=ORIENTED_EDGE('',*,*,#1641,.F.);
#2120=ORIENTED_EDGE('',*,*,#1642,.F.);
#2121=ORIENTED_EDGE('',*,*,#1643,.F.);
#2122=ORIENTED_EDGE('',*,*,#1644,.F.);
#2123=ORIENTED_EDGE('',*,*,#1645,.F.);
#2124=ORIENTED_EDGE('',*,*,#1646,.F.);
#2125=ORIENTED_EDGE('',*,*,#1647,.F.);
#2126=ORIENTED_EDGE('',*,*,#1648,.F.);
#2127=ORIENTED_EDGE('',*,*,#1649,.F.);
#2128=ORIENTED_EDGE('',*,*,#1650,.F.);
#2129=ORIENTED_EDGE('',*,*,#1651,.F.);
#2130=ORIENTED_EDGE('',*,*,#1652,.F.);
#2131=ORIENTED_EDGE('',*,*,#1653,.F.);
#2132=ORIENTED_EDGE('',*,*,#1654,.F.);
#2133=ORIENTED_EDGE('',*,*,#1655,.F.);
#2134=ORIENTED_EDGE('',*,*,#1656,.F.);
#2135=ORIENTED_EDGE('',*,*,#1657,.F.);
#2136=ORIENTED_EDGE('',*,*,#1658,.F.);
#2137=ORIENTED_EDGE('',*,*,#1659,.F.);
#2138=ORIENTED_EDGE('',*,*,#1660,.F.);
#2139=ORIENTED_EDGE('',*,*,#1661,.F.);
#2140=ORIENTED_EDGE('',*,*,#1662,.F.);
#2141=ORIENTED_EDGE('',*,*,#1663,.F.);
#2142=ORIENTED_EDGE('',*,*,#1664,.F.);
#2143=ORIENTED_EDGE('',*,*,#1665,.F.);
#2144=ORIENTED_EDGE('',*,*,#1666,.F.);
#2145=ORIENTED_EDGE('',*,*,#1667,.F.);
#2146=ORIENTED_EDGE('',*,*,#1668,.F.);
#2147=ORIENTED_EDGE('',*,*,#1669,.F.);
#2148=ORIENTED_EDGE('',*,*,#1670,.F.);
#2149=ORIENTED_EDGE('',*,*,#1671,.F.);
#2150=ORIENTED_EDGE('',*,*,#1672,.F.);
#2151=ORIENTED_EDGE('',*,*,#1673,.F.);
#2152=ORIENTED_EDGE('',*,*,#1674,.F.);
#2153=ORIENTED_EDGE('',*,*,#1675,.F.);
#2154=ORIENTED_EDGE('',*,*,#1676,.F.);
#2155=ORIENTED_EDGE('',*,*,#1677,.F.);
#2156=ORIENTED_EDGE('',*,*,#1678,.F.);
#2157=ORIENTED_EDGE('',*,*,#1679,.F.);
#2158=ORIENTED_EDGE('',*,*,#1680,.F.);
#2159=ORIENTED_EDGE('',*,*,#1681,.F.);
#2160=ORIENTED_EDGE('',*,*,#1682,.F.);
#2161=ORIENTED_EDGE('',*,*,#1683,.F.);
#2162=ORIENTED_EDGE('',*,*,#1684,.F.);
#2163=ORIENTED_EDGE('',*,*,#1685,.F.);
#2164=ORIENTED_EDGE('',*,*,#1686,.F.);
#2165=ORIENTED_EDGE('',*,*,#1687,.F.);
#2166=ORIENTED_EDGE('',*,*,#1688,.F.);
#2167=ORIENTED_EDGE('',*,*,#1689,.F.);
#2168=ORIENTED_EDGE('',*,*,#1690,.F.);
#2169=ORIENTED_EDGE('',*,*,#1691,.F.);
#2170=ORIENTED_EDGE('',*,*,#1692,.F.);
#2171=ORIENTED_EDGE('',*,*,#1693,.F.);
#2172=ORIENTED_EDGE('',*,*,#1694,.F.);
#2173=ORIENTED_EDGE('',*,*,#1695,.F.);
#2174=ORIENTED_EDGE('',*,*,#1696,.F.);
#2175=ORIENTED_EDGE('',*,*,#1697,.F.);
#2176=ORIENTED_EDGE('',*,*,#1698,.F.);
#2177=ORIENTED_EDGE('',*,*,#1699,.F.);
#2178=ORIENTED_EDGE('',*,*,#1700,.F.);
#2179=ORIENTED_EDGE('',*,*,#1701,.F.);
#2180=ORIENTED_EDGE('',*,*,#1702,.F.);
#2181=ORIENTED_EDGE('',*,*,#1703,.F.);
#2182=ORIENTED_EDGE('',*,*,#1704,.F.);
#2183=ORIENTED_EDGE('',*,*,#1705,.F.);
#2184=ORIENTED_EDGE('',*,*,#1706,.F.);
#2185=ORIENTED_EDGE('',*,*,#1707,.F.);
#2186=ORIENTED_EDGE('',*,*,#1708,.F.);
#2187=ORIENTED_EDGE('',*,*,#1709,.T.);
#2188=ORIENTED_EDGE('',*,*,#1710,.T.);
#2189=ORIENTED_EDGE('',*,*,#1711,.T.);
#2190=ORIENTED_EDGE('',*,*,#1706,.T.);
#2191=ORIENTED_EDGE('',*,*,#1712,.T.);
#2192=ORIENTED_EDGE('',*,*,#1702,.T.);
#2193=ORIENTED_EDGE('',*,*,#1713,.T.);
#2194=ORIENTED_EDGE('',*,*,#1698,.T.);
#2195=ORIENTED_EDGE('',*,*,#1714,.T.);
#2196=ORIENTED_EDGE('',*,*,#1694,.T.);
#2197=ORIENTED_EDGE('',*,*,#1715,.T.);
#2198=ORIENTED_EDGE('',*,*,#1690,.T.);
#2199=ORIENTED_EDGE('',*,*,#1716,.T.);
#2200=ORIENTED_EDGE('',*,*,#1686,.T.);
#2201=ORIENTED_EDGE('',*,*,#1717,.T.);
#2202=ORIENTED_EDGE('',*,*,#1682,.T.);
#2203=ORIENTED_EDGE('',*,*,#1718,.T.);
#2204=ORIENTED_EDGE('',*,*,#1678,.T.);
#2205=ORIENTED_EDGE('',*,*,#1719,.T.);
#2206=ORIENTED_EDGE('',*,*,#1674,.T.);
#2207=ORIENTED_EDGE('',*,*,#1720,.T.);
#2208=ORIENTED_EDGE('',*,*,#1670,.T.);
#2209=ORIENTED_EDGE('',*,*,#1721,.T.);
#2210=ORIENTED_EDGE('',*,*,#1666,.T.);
#2211=ORIENTED_EDGE('',*,*,#1722,.T.);
#2212=ORIENTED_EDGE('',*,*,#1662,.T.);
#2213=ORIENTED_EDGE('',*,*,#1723,.T.);
#2214=ORIENTED_EDGE('',*,*,#1658,.T.);
#2215=ORIENTED_EDGE('',*,*,#1724,.T.);
#2216=ORIENTED_EDGE('',*,*,#1654,.T.);
#2217=ORIENTED_EDGE('',*,*,#1725,.T.);
#2218=ORIENTED_EDGE('',*,*,#1650,.T.);
#2219=ORIENTED_EDGE('',*,*,#1726,.T.);
#2220=ORIENTED_EDGE('',*,*,#1646,.T.);
#2221=ORIENTED_EDGE('',*,*,#1727,.T.);
#2222=ORIENTED_EDGE('',*,*,#1642,.T.);
#2223=ORIENTED_EDGE('',*,*,#1728,.T.);
#2224=ORIENTED_EDGE('',*,*,#1638,.T.);
#2225=ORIENTED_EDGE('',*,*,#1729,.T.);
#2226=ORIENTED_EDGE('',*,*,#1634,.T.);
#2227=ORIENTED_EDGE('',*,*,#1730,.T.);
#2228=ORIENTED_EDGE('',*,*,#1630,.T.);
#2229=ORIENTED_EDGE('',*,*,#1731,.T.);
#2230=ORIENTED_EDGE('',*,*,#1626,.T.);
#2231=ORIENTED_EDGE('',*,*,#1732,.T.);
#2232=ORIENTED_EDGE('',*,*,#1622,.T.);
#2233=ORIENTED_EDGE('',*,*,#1733,.T.);
#2234=ORIENTED_EDGE('',*,*,#1618,.T.);
#2235=ORIENTED_EDGE('',*,*,#1734,.T.);
#2236=ORIENTED_EDGE('',*,*,#1614,.T.);
#2237=ORIENTED_EDGE('',*,*,#1735,.T.);
#2238=ORIENTED_EDGE('',*,*,#1736,.T.);
#2239=ORIENTED_EDGE('',*,*,#1709,.F.);
#2240=ORIENTED_EDGE('',*,*,#1613,.T.);
#2241=ORIENTED_EDGE('',*,*,#1737,.T.);
#2242=ORIENTED_EDGE('',*,*,#1738,.T.);
#2243=ORIENTED_EDGE('',*,*,#1735,.F.);
#2244=ORIENTED_EDGE('',*,*,#1707,.T.);
#2245=ORIENTED_EDGE('',*,*,#1711,.F.);
#2246=ORIENTED_EDGE('',*,*,#1739,.T.);
#2247=ORIENTED_EDGE('',*,*,#1740,.T.);
#2248=ORIENTED_EDGE('',*,*,#1703,.T.);
#2249=ORIENTED_EDGE('',*,*,#1712,.F.);
#2250=ORIENTED_EDGE('',*,*,#1705,.T.);
#2251=ORIENTED_EDGE('',*,*,#1741,.T.);
#2252=ORIENTED_EDGE('',*,*,#1699,.T.);
#2253=ORIENTED_EDGE('',*,*,#1713,.F.);
#2254=ORIENTED_EDGE('',*,*,#1701,.T.);
#2255=ORIENTED_EDGE('',*,*,#1742,.T.);
#2256=ORIENTED_EDGE('',*,*,#1695,.T.);
#2257=ORIENTED_EDGE('',*,*,#1714,.F.);
#2258=ORIENTED_EDGE('',*,*,#1697,.T.);
#2259=ORIENTED_EDGE('',*,*,#1743,.T.);
#2260=ORIENTED_EDGE('',*,*,#1691,.T.);
#2261=ORIENTED_EDGE('',*,*,#1715,.F.);
#2262=ORIENTED_EDGE('',*,*,#1693,.T.);
#2263=ORIENTED_EDGE('',*,*,#1744,.T.);
#2264=ORIENTED_EDGE('',*,*,#1687,.T.);
#2265=ORIENTED_EDGE('',*,*,#1716,.F.);
#2266=ORIENTED_EDGE('',*,*,#1689,.T.);
#2267=ORIENTED_EDGE('',*,*,#1745,.T.);
#2268=ORIENTED_EDGE('',*,*,#1683,.T.);
#2269=ORIENTED_EDGE('',*,*,#1717,.F.);
#2270=ORIENTED_EDGE('',*,*,#1685,.T.);
#2271=ORIENTED_EDGE('',*,*,#1746,.T.);
#2272=ORIENTED_EDGE('',*,*,#1679,.T.);
#2273=ORIENTED_EDGE('',*,*,#1718,.F.);
#2274=ORIENTED_EDGE('',*,*,#1681,.T.);
#2275=ORIENTED_EDGE('',*,*,#1747,.T.);
#2276=ORIENTED_EDGE('',*,*,#1675,.T.);
#2277=ORIENTED_EDGE('',*,*,#1719,.F.);
#2278=ORIENTED_EDGE('',*,*,#1677,.T.);
#2279=ORIENTED_EDGE('',*,*,#1748,.T.);
#2280=ORIENTED_EDGE('',*,*,#1671,.T.);
#2281=ORIENTED_EDGE('',*,*,#1720,.F.);
#2282=ORIENTED_EDGE('',*,*,#1673,.T.);
#2283=ORIENTED_EDGE('',*,*,#1749,.T.);
#2284=ORIENTED_EDGE('',*,*,#1667,.T.);
#2285=ORIENTED_EDGE('',*,*,#1721,.F.);
#2286=ORIENTED_EDGE('',*,*,#1669,.T.);
#2287=ORIENTED_EDGE('',*,*,#1750,.T.);
#2288=ORIENTED_EDGE('',*,*,#1663,.T.);
#2289=ORIENTED_EDGE('',*,*,#1722,.F.);
#2290=ORIENTED_EDGE('',*,*,#1665,.T.);
#2291=ORIENTED_EDGE('',*,*,#1751,.T.);
#2292=ORIENTED_EDGE('',*,*,#1659,.T.);
#2293=ORIENTED_EDGE('',*,*,#1723,.F.);
#2294=ORIENTED_EDGE('',*,*,#1661,.T.);
#2295=ORIENTED_EDGE('',*,*,#1752,.T.);
#2296=ORIENTED_EDGE('',*,*,#1655,.T.);
#2297=ORIENTED_EDGE('',*,*,#1724,.F.);
#2298=ORIENTED_EDGE('',*,*,#1657,.T.);
#2299=ORIENTED_EDGE('',*,*,#1753,.T.);
#2300=ORIENTED_EDGE('',*,*,#1651,.T.);
#2301=ORIENTED_EDGE('',*,*,#1725,.F.);
#2302=ORIENTED_EDGE('',*,*,#1653,.T.);
#2303=ORIENTED_EDGE('',*,*,#1754,.T.);
#2304=ORIENTED_EDGE('',*,*,#1647,.T.);
#2305=ORIENTED_EDGE('',*,*,#1726,.F.);
#2306=ORIENTED_EDGE('',*,*,#1649,.T.);
#2307=ORIENTED_EDGE('',*,*,#1755,.T.);
#2308=ORIENTED_EDGE('',*,*,#1643,.T.);
#2309=ORIENTED_EDGE('',*,*,#1727,.F.);
#2310=ORIENTED_EDGE('',*,*,#1645,.T.);
#2311=ORIENTED_EDGE('',*,*,#1756,.T.);
#2312=ORIENTED_EDGE('',*,*,#1639,.T.);
#2313=ORIENTED_EDGE('',*,*,#1728,.F.);
#2314=ORIENTED_EDGE('',*,*,#1641,.T.);
#2315=ORIENTED_EDGE('',*,*,#1757,.T.);
#2316=ORIENTED_EDGE('',*,*,#1635,.T.);
#2317=ORIENTED_EDGE('',*,*,#1729,.F.);
#2318=ORIENTED_EDGE('',*,*,#1637,.T.);
#2319=ORIENTED_EDGE('',*,*,#1758,.T.);
#2320=ORIENTED_EDGE('',*,*,#1631,.T.);
#2321=ORIENTED_EDGE('',*,*,#1730,.F.);
#2322=ORIENTED_EDGE('',*,*,#1633,.T.);
#2323=ORIENTED_EDGE('',*,*,#1759,.T.);
#2324=ORIENTED_EDGE('',*,*,#1627,.T.);
#2325=ORIENTED_EDGE('',*,*,#1731,.F.);
#2326=ORIENTED_EDGE('',*,*,#1629,.T.);
#2327=ORIENTED_EDGE('',*,*,#1760,.T.);
#2328=ORIENTED_EDGE('',*,*,#1623,.T.);
#2329=ORIENTED_EDGE('',*,*,#1732,.F.);
#2330=ORIENTED_EDGE('',*,*,#1625,.T.);
#2331=ORIENTED_EDGE('',*,*,#1761,.T.);
#2332=ORIENTED_EDGE('',*,*,#1619,.T.);
#2333=ORIENTED_EDGE('',*,*,#1733,.F.);
#2334=ORIENTED_EDGE('',*,*,#1621,.T.);
#2335=ORIENTED_EDGE('',*,*,#1762,.T.);
#2336=ORIENTED_EDGE('',*,*,#1763,.F.);
#2337=ORIENTED_EDGE('',*,*,#1739,.F.);
#2338=ORIENTED_EDGE('',*,*,#1710,.F.);
#2339=ORIENTED_EDGE('',*,*,#1736,.F.);
#2340=ORIENTED_EDGE('',*,*,#1738,.F.);
#2341=ORIENTED_EDGE('',*,*,#1764,.F.);
#2342=ORIENTED_EDGE('',*,*,#1612,.T.);
#2343=ORIENTED_EDGE('',*,*,#1765,.F.);
#2344=ORIENTED_EDGE('',*,*,#1616,.T.);
#2345=ORIENTED_EDGE('',*,*,#1762,.F.);
#2346=ORIENTED_EDGE('',*,*,#1620,.T.);
#2347=ORIENTED_EDGE('',*,*,#1761,.F.);
#2348=ORIENTED_EDGE('',*,*,#1624,.T.);
#2349=ORIENTED_EDGE('',*,*,#1760,.F.);
#2350=ORIENTED_EDGE('',*,*,#1628,.T.);
#2351=ORIENTED_EDGE('',*,*,#1759,.F.);
#2352=ORIENTED_EDGE('',*,*,#1632,.T.);
#2353=ORIENTED_EDGE('',*,*,#1758,.F.);
#2354=ORIENTED_EDGE('',*,*,#1636,.T.);
#2355=ORIENTED_EDGE('',*,*,#1757,.F.);
#2356=ORIENTED_EDGE('',*,*,#1640,.T.);
#2357=ORIENTED_EDGE('',*,*,#1756,.F.);
#2358=ORIENTED_EDGE('',*,*,#1644,.T.);
#2359=ORIENTED_EDGE('',*,*,#1755,.F.);
#2360=ORIENTED_EDGE('',*,*,#1648,.T.);
#2361=ORIENTED_EDGE('',*,*,#1754,.F.);
#2362=ORIENTED_EDGE('',*,*,#1652,.T.);
#2363=ORIENTED_EDGE('',*,*,#1753,.F.);
#2364=ORIENTED_EDGE('',*,*,#1656,.T.);
#2365=ORIENTED_EDGE('',*,*,#1752,.F.);
#2366=ORIENTED_EDGE('',*,*,#1660,.T.);
#2367=ORIENTED_EDGE('',*,*,#1751,.F.);
#2368=ORIENTED_EDGE('',*,*,#1664,.T.);
#2369=ORIENTED_EDGE('',*,*,#1750,.F.);
#2370=ORIENTED_EDGE('',*,*,#1668,.T.);
#2371=ORIENTED_EDGE('',*,*,#1749,.F.);
#2372=ORIENTED_EDGE('',*,*,#1672,.T.);
#2373=ORIENTED_EDGE('',*,*,#1748,.F.);
#2374=ORIENTED_EDGE('',*,*,#1676,.T.);
#2375=ORIENTED_EDGE('',*,*,#1747,.F.);
#2376=ORIENTED_EDGE('',*,*,#1680,.T.);
#2377=ORIENTED_EDGE('',*,*,#1746,.F.);
#2378=ORIENTED_EDGE('',*,*,#1684,.T.);
#2379=ORIENTED_EDGE('',*,*,#1745,.F.);
#2380=ORIENTED_EDGE('',*,*,#1688,.T.);
#2381=ORIENTED_EDGE('',*,*,#1744,.F.);
#2382=ORIENTED_EDGE('',*,*,#1692,.T.);
#2383=ORIENTED_EDGE('',*,*,#1743,.F.);
#2384=ORIENTED_EDGE('',*,*,#1696,.T.);
#2385=ORIENTED_EDGE('',*,*,#1742,.F.);
#2386=ORIENTED_EDGE('',*,*,#1700,.T.);
#2387=ORIENTED_EDGE('',*,*,#1741,.F.);
#2388=ORIENTED_EDGE('',*,*,#1704,.T.);
#2389=ORIENTED_EDGE('',*,*,#1740,.F.);
#2390=ORIENTED_EDGE('',*,*,#1763,.T.);
#2391=ORIENTED_EDGE('',*,*,#1766,.T.);
#2392=ORIENTED_EDGE('',*,*,#1610,.T.);
#2393=ORIENTED_EDGE('',*,*,#1766,.F.);
#2394=ORIENTED_EDGE('',*,*,#1764,.T.);
#2395=ORIENTED_EDGE('',*,*,#1737,.F.);
#2396=ORIENTED_EDGE('',*,*,#1615,.T.);
#2397=ORIENTED_EDGE('',*,*,#1734,.F.);
#2398=ORIENTED_EDGE('',*,*,#1617,.T.);
#2399=ORIENTED_EDGE('',*,*,#1765,.T.);
#2400=ORIENTED_EDGE('',*,*,#1708,.T.);
#2401=ORIENTED_EDGE('',*,*,#1767,.F.);
#2402=ORIENTED_EDGE('',*,*,#1767,.T.);
#2403=ORIENTED_EDGE('',*,*,#1768,.T.);
#2404=ORIENTED_EDGE('',*,*,#1609,.F.);
#2405=ORIENTED_EDGE('',*,*,#1768,.F.);
#2406=ORIENTED_EDGE('',*,*,#1769,.T.);
#2407=ORIENTED_EDGE('',*,*,#1770,.T.);
#2408=ORIENTED_EDGE('',*,*,#1771,.T.);
#2409=ORIENTED_EDGE('',*,*,#1772,.T.);
#2410=ORIENTED_EDGE('',*,*,#1770,.F.);
#2411=ORIENTED_EDGE('',*,*,#1773,.T.);
#2412=ORIENTED_EDGE('',*,*,#1774,.T.);
#2413=ORIENTED_EDGE('',*,*,#1775,.T.);
#2414=ORIENTED_EDGE('',*,*,#1769,.F.);
#2415=ORIENTED_EDGE('',*,*,#1776,.F.);
#2416=ORIENTED_EDGE('',*,*,#1777,.F.);
#2417=ORIENTED_EDGE('',*,*,#1778,.T.);
#2418=ORIENTED_EDGE('',*,*,#1779,.T.);
#2419=ORIENTED_EDGE('',*,*,#1773,.F.);
#2420=ORIENTED_EDGE('',*,*,#1780,.T.);
#2421=ORIENTED_EDGE('',*,*,#1781,.T.);
#2422=ORIENTED_EDGE('',*,*,#1777,.T.);
#2423=ORIENTED_EDGE('',*,*,#1782,.T.);
#2424=ORIENTED_EDGE('',*,*,#1772,.F.);
#2425=ORIENTED_EDGE('',*,*,#1783,.F.);
#2426=ORIENTED_EDGE('',*,*,#1782,.F.);
#2427=ORIENTED_EDGE('',*,*,#1776,.T.);
#2428=ORIENTED_EDGE('',*,*,#1771,.F.);
#2429=ORIENTED_EDGE('',*,*,#1775,.F.);
#2430=ORIENTED_EDGE('',*,*,#1784,.F.);
#2431=ORIENTED_EDGE('',*,*,#1785,.T.);
#2432=ORIENTED_EDGE('',*,*,#1780,.F.);
#2433=ORIENTED_EDGE('',*,*,#1783,.T.);
#2434=ORIENTED_EDGE('',*,*,#1786,.T.);
#2435=ORIENTED_EDGE('',*,*,#1784,.T.);
#2436=ORIENTED_EDGE('',*,*,#1774,.F.);
#2437=ORIENTED_EDGE('',*,*,#1779,.F.);
#2438=ORIENTED_EDGE('',*,*,#1781,.F.);
#2439=ORIENTED_EDGE('',*,*,#1785,.F.);
#2440=ORIENTED_EDGE('',*,*,#1786,.F.);
#2441=ORIENTED_EDGE('',*,*,#1778,.F.);
#2442=ORIENTED_EDGE('',*,*,#1787,.F.);
#2443=ORIENTED_EDGE('',*,*,#1788,.F.);
#2444=ORIENTED_EDGE('',*,*,#1789,.F.);
#2445=ORIENTED_EDGE('',*,*,#1790,.F.);
#2446=ORIENTED_EDGE('',*,*,#1791,.F.);
#2447=ORIENTED_EDGE('',*,*,#1792,.F.);
#2448=ORIENTED_EDGE('',*,*,#1793,.F.);
#2449=ORIENTED_EDGE('',*,*,#1794,.F.);
#2450=ORIENTED_EDGE('',*,*,#1795,.F.);
#2451=ORIENTED_EDGE('',*,*,#1796,.F.);
#2452=ORIENTED_EDGE('',*,*,#1797,.F.);
#2453=ORIENTED_EDGE('',*,*,#1798,.F.);
#2454=ORIENTED_EDGE('',*,*,#1799,.F.);
#2455=ORIENTED_EDGE('',*,*,#1800,.F.);
#2456=ORIENTED_EDGE('',*,*,#1801,.F.);
#2457=ORIENTED_EDGE('',*,*,#1802,.F.);
#2458=ORIENTED_EDGE('',*,*,#1803,.F.);
#2459=ORIENTED_EDGE('',*,*,#1804,.F.);
#2460=ORIENTED_EDGE('',*,*,#1805,.F.);
#2461=ORIENTED_EDGE('',*,*,#1806,.F.);
#2462=ORIENTED_EDGE('',*,*,#1807,.F.);
#2463=ORIENTED_EDGE('',*,*,#1808,.F.);
#2464=ORIENTED_EDGE('',*,*,#1809,.F.);
#2465=ORIENTED_EDGE('',*,*,#1810,.F.);
#2466=ORIENTED_EDGE('',*,*,#1811,.F.);
#2467=ORIENTED_EDGE('',*,*,#1812,.F.);
#2468=ORIENTED_EDGE('',*,*,#1813,.F.);
#2469=ORIENTED_EDGE('',*,*,#1814,.F.);
#2470=ORIENTED_EDGE('',*,*,#1815,.F.);
#2471=ORIENTED_EDGE('',*,*,#1816,.F.);
#2472=ORIENTED_EDGE('',*,*,#1817,.F.);
#2473=ORIENTED_EDGE('',*,*,#1818,.F.);
#2474=ORIENTED_EDGE('',*,*,#1819,.F.);
#2475=ORIENTED_EDGE('',*,*,#1820,.F.);
#2476=ORIENTED_EDGE('',*,*,#1821,.F.);
#2477=ORIENTED_EDGE('',*,*,#1822,.F.);
#2478=ORIENTED_EDGE('',*,*,#1790,.T.);
#2479=ORIENTED_EDGE('',*,*,#1823,.F.);
#2480=ORIENTED_EDGE('',*,*,#1794,.T.);
#2481=ORIENTED_EDGE('',*,*,#1824,.F.);
#2482=ORIENTED_EDGE('',*,*,#1798,.T.);
#2483=ORIENTED_EDGE('',*,*,#1825,.F.);
#2484=ORIENTED_EDGE('',*,*,#1802,.T.);
#2485=ORIENTED_EDGE('',*,*,#1826,.F.);
#2486=ORIENTED_EDGE('',*,*,#1806,.T.);
#2487=ORIENTED_EDGE('',*,*,#1827,.F.);
#2488=ORIENTED_EDGE('',*,*,#1810,.T.);
#2489=ORIENTED_EDGE('',*,*,#1828,.F.);
#2490=ORIENTED_EDGE('',*,*,#1814,.T.);
#2491=ORIENTED_EDGE('',*,*,#1829,.F.);
#2492=ORIENTED_EDGE('',*,*,#1818,.T.);
#2493=ORIENTED_EDGE('',*,*,#1830,.F.);
#2494=ORIENTED_EDGE('',*,*,#1822,.T.);
#2495=ORIENTED_EDGE('',*,*,#1831,.F.);
#2496=ORIENTED_EDGE('',*,*,#1832,.T.);
#2497=ORIENTED_EDGE('',*,*,#1833,.F.);
#2498=ORIENTED_EDGE('',*,*,#1834,.T.);
#2499=ORIENTED_EDGE('',*,*,#1821,.T.);
#2500=ORIENTED_EDGE('',*,*,#1835,.F.);
#2501=ORIENTED_EDGE('',*,*,#1836,.T.);
#2502=ORIENTED_EDGE('',*,*,#1831,.T.);
#2503=ORIENTED_EDGE('',*,*,#1817,.T.);
#2504=ORIENTED_EDGE('',*,*,#1837,.F.);
#2505=ORIENTED_EDGE('',*,*,#1819,.T.);
#2506=ORIENTED_EDGE('',*,*,#1830,.T.);
#2507=ORIENTED_EDGE('',*,*,#1813,.T.);
#2508=ORIENTED_EDGE('',*,*,#1838,.F.);
#2509=ORIENTED_EDGE('',*,*,#1815,.T.);
#2510=ORIENTED_EDGE('',*,*,#1829,.T.);
#2511=ORIENTED_EDGE('',*,*,#1809,.T.);
#2512=ORIENTED_EDGE('',*,*,#1839,.F.);
#2513=ORIENTED_EDGE('',*,*,#1811,.T.);
#2514=ORIENTED_EDGE('',*,*,#1828,.T.);
#2515=ORIENTED_EDGE('',*,*,#1805,.T.);
#2516=ORIENTED_EDGE('',*,*,#1840,.F.);
#2517=ORIENTED_EDGE('',*,*,#1807,.T.);
#2518=ORIENTED_EDGE('',*,*,#1827,.T.);
#2519=ORIENTED_EDGE('',*,*,#1801,.T.);
#2520=ORIENTED_EDGE('',*,*,#1841,.F.);
#2521=ORIENTED_EDGE('',*,*,#1803,.T.);
#2522=ORIENTED_EDGE('',*,*,#1826,.T.);
#2523=ORIENTED_EDGE('',*,*,#1797,.T.);
#2524=ORIENTED_EDGE('',*,*,#1842,.F.);
#2525=ORIENTED_EDGE('',*,*,#1799,.T.);
#2526=ORIENTED_EDGE('',*,*,#1825,.T.);
#2527=ORIENTED_EDGE('',*,*,#1793,.T.);
#2528=ORIENTED_EDGE('',*,*,#1843,.F.);
#2529=ORIENTED_EDGE('',*,*,#1795,.T.);
#2530=ORIENTED_EDGE('',*,*,#1824,.T.);
#2531=ORIENTED_EDGE('',*,*,#1789,.T.);
#2532=ORIENTED_EDGE('',*,*,#1844,.F.);
#2533=ORIENTED_EDGE('',*,*,#1791,.T.);
#2534=ORIENTED_EDGE('',*,*,#1823,.T.);
#2535=ORIENTED_EDGE('',*,*,#1845,.T.);
#2536=ORIENTED_EDGE('',*,*,#1846,.T.);
#2537=ORIENTED_EDGE('',*,*,#1847,.T.);
#2538=ORIENTED_EDGE('',*,*,#1835,.T.);
#2539=ORIENTED_EDGE('',*,*,#1820,.T.);
#2540=ORIENTED_EDGE('',*,*,#1837,.T.);
#2541=ORIENTED_EDGE('',*,*,#1816,.T.);
#2542=ORIENTED_EDGE('',*,*,#1838,.T.);
#2543=ORIENTED_EDGE('',*,*,#1812,.T.);
#2544=ORIENTED_EDGE('',*,*,#1839,.T.);
#2545=ORIENTED_EDGE('',*,*,#1808,.T.);
#2546=ORIENTED_EDGE('',*,*,#1840,.T.);
#2547=ORIENTED_EDGE('',*,*,#1804,.T.);
#2548=ORIENTED_EDGE('',*,*,#1841,.T.);
#2549=ORIENTED_EDGE('',*,*,#1800,.T.);
#2550=ORIENTED_EDGE('',*,*,#1842,.T.);
#2551=ORIENTED_EDGE('',*,*,#1796,.T.);
#2552=ORIENTED_EDGE('',*,*,#1843,.T.);
#2553=ORIENTED_EDGE('',*,*,#1792,.T.);
#2554=ORIENTED_EDGE('',*,*,#1844,.T.);
#2555=ORIENTED_EDGE('',*,*,#1788,.T.);
#2556=ORIENTED_EDGE('',*,*,#1848,.T.);
#2557=ORIENTED_EDGE('',*,*,#1849,.T.);
#2558=ORIENTED_EDGE('',*,*,#1846,.F.);
#2559=ORIENTED_EDGE('',*,*,#1836,.F.);
#2560=ORIENTED_EDGE('',*,*,#1847,.F.);
#2561=ORIENTED_EDGE('',*,*,#1849,.F.);
#2562=ORIENTED_EDGE('',*,*,#1850,.F.);
#2563=ORIENTED_EDGE('',*,*,#1832,.F.);
#2564=ORIENTED_EDGE('',*,*,#1787,.T.);
#2565=ORIENTED_EDGE('',*,*,#1833,.T.);
#2566=ORIENTED_EDGE('',*,*,#1850,.T.);
#2567=ORIENTED_EDGE('',*,*,#1848,.F.);
#2568=ORIENTED_EDGE('',*,*,#1845,.F.);
#2569=ORIENTED_EDGE('',*,*,#1851,.F.);
#2570=ORIENTED_EDGE('',*,*,#1852,.T.);
#2571=ORIENTED_EDGE('',*,*,#1834,.F.);
#2572=ORIENTED_EDGE('',*,*,#1852,.F.);
#2573=ORIENTED_EDGE('',*,*,#1851,.T.);
#2574=ORIENTED_EDGE('',*,*,#1853,.F.);
#2575=ORIENTED_EDGE('',*,*,#1854,.F.);
#2576=ORIENTED_EDGE('',*,*,#1855,.F.);
#2577=ORIENTED_EDGE('',*,*,#1856,.F.);
#2578=ORIENTED_EDGE('',*,*,#1857,.F.);
#2579=ORIENTED_EDGE('',*,*,#1858,.F.);
#2580=ORIENTED_EDGE('',*,*,#1859,.F.);
#2581=ORIENTED_EDGE('',*,*,#1860,.F.);
#2582=ORIENTED_EDGE('',*,*,#1861,.F.);
#2583=ORIENTED_EDGE('',*,*,#1862,.F.);
#2584=ORIENTED_EDGE('',*,*,#1863,.F.);
#2585=ORIENTED_EDGE('',*,*,#1864,.F.);
#2586=ORIENTED_EDGE('',*,*,#1865,.F.);
#2587=ORIENTED_EDGE('',*,*,#1866,.F.);
#2588=ORIENTED_EDGE('',*,*,#1867,.F.);
#2589=ORIENTED_EDGE('',*,*,#1868,.F.);
#2590=ORIENTED_EDGE('',*,*,#1869,.F.);
#2591=ORIENTED_EDGE('',*,*,#1870,.F.);
#2592=ORIENTED_EDGE('',*,*,#1871,.F.);
#2593=ORIENTED_EDGE('',*,*,#1872,.F.);
#2594=ORIENTED_EDGE('',*,*,#1873,.F.);
#2595=ORIENTED_EDGE('',*,*,#1874,.F.);
#2596=ORIENTED_EDGE('',*,*,#1875,.F.);
#2597=ORIENTED_EDGE('',*,*,#1876,.F.);
#2598=ORIENTED_EDGE('',*,*,#1877,.F.);
#2599=ORIENTED_EDGE('',*,*,#1878,.F.);
#2600=ORIENTED_EDGE('',*,*,#1879,.F.);
#2601=ORIENTED_EDGE('',*,*,#1880,.F.);
#2602=ORIENTED_EDGE('',*,*,#1881,.F.);
#2603=ORIENTED_EDGE('',*,*,#1882,.F.);
#2604=ORIENTED_EDGE('',*,*,#1883,.F.);
#2605=ORIENTED_EDGE('',*,*,#1884,.F.);
#2606=ORIENTED_EDGE('',*,*,#1885,.F.);
#2607=ORIENTED_EDGE('',*,*,#1886,.F.);
#2608=ORIENTED_EDGE('',*,*,#1887,.F.);
#2609=ORIENTED_EDGE('',*,*,#1888,.F.);
#2610=ORIENTED_EDGE('',*,*,#1889,.F.);
#2611=ORIENTED_EDGE('',*,*,#1890,.F.);
#2612=ORIENTED_EDGE('',*,*,#1891,.F.);
#2613=ORIENTED_EDGE('',*,*,#1892,.F.);
#2614=ORIENTED_EDGE('',*,*,#1893,.F.);
#2615=ORIENTED_EDGE('',*,*,#1894,.F.);
#2616=ORIENTED_EDGE('',*,*,#1895,.F.);
#2617=ORIENTED_EDGE('',*,*,#1896,.F.);
#2618=ORIENTED_EDGE('',*,*,#1897,.F.);
#2619=ORIENTED_EDGE('',*,*,#1898,.F.);
#2620=ORIENTED_EDGE('',*,*,#1899,.F.);
#2621=ORIENTED_EDGE('',*,*,#1900,.F.);
#2622=ORIENTED_EDGE('',*,*,#1901,.F.);
#2623=ORIENTED_EDGE('',*,*,#1902,.F.);
#2624=ORIENTED_EDGE('',*,*,#1903,.F.);
#2625=ORIENTED_EDGE('',*,*,#1904,.F.);
#2626=ORIENTED_EDGE('',*,*,#1905,.F.);
#2627=ORIENTED_EDGE('',*,*,#1906,.F.);
#2628=ORIENTED_EDGE('',*,*,#1907,.F.);
#2629=ORIENTED_EDGE('',*,*,#1908,.F.);
#2630=ORIENTED_EDGE('',*,*,#1909,.F.);
#2631=ORIENTED_EDGE('',*,*,#1910,.F.);
#2632=ORIENTED_EDGE('',*,*,#1911,.F.);
#2633=ORIENTED_EDGE('',*,*,#1912,.F.);
#2634=ORIENTED_EDGE('',*,*,#1913,.F.);
#2635=ORIENTED_EDGE('',*,*,#1914,.F.);
#2636=ORIENTED_EDGE('',*,*,#1915,.F.);
#2637=ORIENTED_EDGE('',*,*,#1916,.F.);
#2638=ORIENTED_EDGE('',*,*,#1917,.F.);
#2639=ORIENTED_EDGE('',*,*,#1918,.F.);
#2640=ORIENTED_EDGE('',*,*,#1919,.F.);
#2641=ORIENTED_EDGE('',*,*,#1920,.F.);
#2642=ORIENTED_EDGE('',*,*,#1921,.F.);
#2643=ORIENTED_EDGE('',*,*,#1922,.F.);
#2644=ORIENTED_EDGE('',*,*,#1923,.F.);
#2645=ORIENTED_EDGE('',*,*,#1924,.F.);
#2646=ORIENTED_EDGE('',*,*,#1925,.F.);
#2647=ORIENTED_EDGE('',*,*,#1926,.F.);
#2648=ORIENTED_EDGE('',*,*,#1927,.F.);
#2649=ORIENTED_EDGE('',*,*,#1928,.F.);
#2650=ORIENTED_EDGE('',*,*,#1929,.F.);
#2651=ORIENTED_EDGE('',*,*,#1930,.F.);
#2652=ORIENTED_EDGE('',*,*,#1931,.F.);
#2653=ORIENTED_EDGE('',*,*,#1932,.F.);
#2654=ORIENTED_EDGE('',*,*,#1933,.F.);
#2655=ORIENTED_EDGE('',*,*,#1934,.F.);
#2656=ORIENTED_EDGE('',*,*,#1935,.F.);
#2657=ORIENTED_EDGE('',*,*,#1936,.F.);
#2658=ORIENTED_EDGE('',*,*,#1937,.F.);
#2659=ORIENTED_EDGE('',*,*,#1938,.F.);
#2660=ORIENTED_EDGE('',*,*,#1939,.F.);
#2661=ORIENTED_EDGE('',*,*,#1940,.F.);
#2662=ORIENTED_EDGE('',*,*,#1941,.F.);
#2663=ORIENTED_EDGE('',*,*,#1942,.F.);
#2664=ORIENTED_EDGE('',*,*,#1943,.F.);
#2665=ORIENTED_EDGE('',*,*,#1944,.F.);
#2666=ORIENTED_EDGE('',*,*,#1945,.F.);
#2667=ORIENTED_EDGE('',*,*,#1946,.F.);
#2668=ORIENTED_EDGE('',*,*,#1947,.F.);
#2669=ORIENTED_EDGE('',*,*,#1948,.F.);
#2670=ORIENTED_EDGE('',*,*,#1949,.F.);
#2671=ORIENTED_EDGE('',*,*,#1950,.T.);
#2672=ORIENTED_EDGE('',*,*,#1951,.T.);
#2673=ORIENTED_EDGE('',*,*,#1952,.T.);
#2674=ORIENTED_EDGE('',*,*,#1947,.T.);
#2675=ORIENTED_EDGE('',*,*,#1953,.T.);
#2676=ORIENTED_EDGE('',*,*,#1943,.T.);
#2677=ORIENTED_EDGE('',*,*,#1954,.T.);
#2678=ORIENTED_EDGE('',*,*,#1939,.T.);
#2679=ORIENTED_EDGE('',*,*,#1955,.T.);
#2680=ORIENTED_EDGE('',*,*,#1935,.T.);
#2681=ORIENTED_EDGE('',*,*,#1956,.T.);
#2682=ORIENTED_EDGE('',*,*,#1931,.T.);
#2683=ORIENTED_EDGE('',*,*,#1957,.T.);
#2684=ORIENTED_EDGE('',*,*,#1927,.T.);
#2685=ORIENTED_EDGE('',*,*,#1958,.T.);
#2686=ORIENTED_EDGE('',*,*,#1923,.T.);
#2687=ORIENTED_EDGE('',*,*,#1959,.T.);
#2688=ORIENTED_EDGE('',*,*,#1919,.T.);
#2689=ORIENTED_EDGE('',*,*,#1960,.T.);
#2690=ORIENTED_EDGE('',*,*,#1915,.T.);
#2691=ORIENTED_EDGE('',*,*,#1961,.T.);
#2692=ORIENTED_EDGE('',*,*,#1911,.T.);
#2693=ORIENTED_EDGE('',*,*,#1962,.T.);
#2694=ORIENTED_EDGE('',*,*,#1907,.T.);
#2695=ORIENTED_EDGE('',*,*,#1963,.T.);
#2696=ORIENTED_EDGE('',*,*,#1903,.T.);
#2697=ORIENTED_EDGE('',*,*,#1964,.T.);
#2698=ORIENTED_EDGE('',*,*,#1899,.T.);
#2699=ORIENTED_EDGE('',*,*,#1965,.T.);
#2700=ORIENTED_EDGE('',*,*,#1895,.T.);
#2701=ORIENTED_EDGE('',*,*,#1966,.T.);
#2702=ORIENTED_EDGE('',*,*,#1891,.T.);
#2703=ORIENTED_EDGE('',*,*,#1967,.T.);
#2704=ORIENTED_EDGE('',*,*,#1887,.T.);
#2705=ORIENTED_EDGE('',*,*,#1968,.T.);
#2706=ORIENTED_EDGE('',*,*,#1883,.T.);
#2707=ORIENTED_EDGE('',*,*,#1969,.T.);
#2708=ORIENTED_EDGE('',*,*,#1879,.T.);
#2709=ORIENTED_EDGE('',*,*,#1970,.T.);
#2710=ORIENTED_EDGE('',*,*,#1875,.T.);
#2711=ORIENTED_EDGE('',*,*,#1971,.T.);
#2712=ORIENTED_EDGE('',*,*,#1871,.T.);
#2713=ORIENTED_EDGE('',*,*,#1972,.T.);
#2714=ORIENTED_EDGE('',*,*,#1867,.T.);
#2715=ORIENTED_EDGE('',*,*,#1973,.T.);
#2716=ORIENTED_EDGE('',*,*,#1863,.T.);
#2717=ORIENTED_EDGE('',*,*,#1974,.T.);
#2718=ORIENTED_EDGE('',*,*,#1859,.T.);
#2719=ORIENTED_EDGE('',*,*,#1975,.T.);
#2720=ORIENTED_EDGE('',*,*,#1855,.T.);
#2721=ORIENTED_EDGE('',*,*,#1976,.T.);
#2722=ORIENTED_EDGE('',*,*,#1977,.T.);
#2723=ORIENTED_EDGE('',*,*,#1950,.F.);
#2724=ORIENTED_EDGE('',*,*,#1854,.T.);
#2725=ORIENTED_EDGE('',*,*,#1978,.T.);
#2726=ORIENTED_EDGE('',*,*,#1979,.T.);
#2727=ORIENTED_EDGE('',*,*,#1976,.F.);
#2728=ORIENTED_EDGE('',*,*,#1948,.T.);
#2729=ORIENTED_EDGE('',*,*,#1952,.F.);
#2730=ORIENTED_EDGE('',*,*,#1980,.T.);
#2731=ORIENTED_EDGE('',*,*,#1981,.T.);
#2732=ORIENTED_EDGE('',*,*,#1944,.T.);
#2733=ORIENTED_EDGE('',*,*,#1953,.F.);
#2734=ORIENTED_EDGE('',*,*,#1946,.T.);
#2735=ORIENTED_EDGE('',*,*,#1982,.T.);
#2736=ORIENTED_EDGE('',*,*,#1940,.T.);
#2737=ORIENTED_EDGE('',*,*,#1954,.F.);
#2738=ORIENTED_EDGE('',*,*,#1942,.T.);
#2739=ORIENTED_EDGE('',*,*,#1983,.T.);
#2740=ORIENTED_EDGE('',*,*,#1936,.T.);
#2741=ORIENTED_EDGE('',*,*,#1955,.F.);
#2742=ORIENTED_EDGE('',*,*,#1938,.T.);
#2743=ORIENTED_EDGE('',*,*,#1984,.T.);
#2744=ORIENTED_EDGE('',*,*,#1932,.T.);
#2745=ORIENTED_EDGE('',*,*,#1956,.F.);
#2746=ORIENTED_EDGE('',*,*,#1934,.T.);
#2747=ORIENTED_EDGE('',*,*,#1985,.T.);
#2748=ORIENTED_EDGE('',*,*,#1928,.T.);
#2749=ORIENTED_EDGE('',*,*,#1957,.F.);
#2750=ORIENTED_EDGE('',*,*,#1930,.T.);
#2751=ORIENTED_EDGE('',*,*,#1986,.T.);
#2752=ORIENTED_EDGE('',*,*,#1924,.T.);
#2753=ORIENTED_EDGE('',*,*,#1958,.F.);
#2754=ORIENTED_EDGE('',*,*,#1926,.T.);
#2755=ORIENTED_EDGE('',*,*,#1987,.T.);
#2756=ORIENTED_EDGE('',*,*,#1920,.T.);
#2757=ORIENTED_EDGE('',*,*,#1959,.F.);
#2758=ORIENTED_EDGE('',*,*,#1922,.T.);
#2759=ORIENTED_EDGE('',*,*,#1988,.T.);
#2760=ORIENTED_EDGE('',*,*,#1916,.T.);
#2761=ORIENTED_EDGE('',*,*,#1960,.F.);
#2762=ORIENTED_EDGE('',*,*,#1918,.T.);
#2763=ORIENTED_EDGE('',*,*,#1989,.T.);
#2764=ORIENTED_EDGE('',*,*,#1912,.T.);
#2765=ORIENTED_EDGE('',*,*,#1961,.F.);
#2766=ORIENTED_EDGE('',*,*,#1914,.T.);
#2767=ORIENTED_EDGE('',*,*,#1990,.T.);
#2768=ORIENTED_EDGE('',*,*,#1908,.T.);
#2769=ORIENTED_EDGE('',*,*,#1962,.F.);
#2770=ORIENTED_EDGE('',*,*,#1910,.T.);
#2771=ORIENTED_EDGE('',*,*,#1991,.T.);
#2772=ORIENTED_EDGE('',*,*,#1904,.T.);
#2773=ORIENTED_EDGE('',*,*,#1963,.F.);
#2774=ORIENTED_EDGE('',*,*,#1906,.T.);
#2775=ORIENTED_EDGE('',*,*,#1992,.T.);
#2776=ORIENTED_EDGE('',*,*,#1900,.T.);
#2777=ORIENTED_EDGE('',*,*,#1964,.F.);
#2778=ORIENTED_EDGE('',*,*,#1902,.T.);
#2779=ORIENTED_EDGE('',*,*,#1993,.T.);
#2780=ORIENTED_EDGE('',*,*,#1896,.T.);
#2781=ORIENTED_EDGE('',*,*,#1965,.F.);
#2782=ORIENTED_EDGE('',*,*,#1898,.T.);
#2783=ORIENTED_EDGE('',*,*,#1994,.T.);
#2784=ORIENTED_EDGE('',*,*,#1892,.T.);
#2785=ORIENTED_EDGE('',*,*,#1966,.F.);
#2786=ORIENTED_EDGE('',*,*,#1894,.T.);
#2787=ORIENTED_EDGE('',*,*,#1995,.T.);
#2788=ORIENTED_EDGE('',*,*,#1888,.T.);
#2789=ORIENTED_EDGE('',*,*,#1967,.F.);
#2790=ORIENTED_EDGE('',*,*,#1890,.T.);
#2791=ORIENTED_EDGE('',*,*,#1996,.T.);
#2792=ORIENTED_EDGE('',*,*,#1884,.T.);
#2793=ORIENTED_EDGE('',*,*,#1968,.F.);
#2794=ORIENTED_EDGE('',*,*,#1886,.T.);
#2795=ORIENTED_EDGE('',*,*,#1997,.T.);
#2796=ORIENTED_EDGE('',*,*,#1880,.T.);
#2797=ORIENTED_EDGE('',*,*,#1969,.F.);
#2798=ORIENTED_EDGE('',*,*,#1882,.T.);
#2799=ORIENTED_EDGE('',*,*,#1998,.T.);
#2800=ORIENTED_EDGE('',*,*,#1876,.T.);
#2801=ORIENTED_EDGE('',*,*,#1970,.F.);
#2802=ORIENTED_EDGE('',*,*,#1878,.T.);
#2803=ORIENTED_EDGE('',*,*,#1999,.T.);
#2804=ORIENTED_EDGE('',*,*,#1872,.T.);
#2805=ORIENTED_EDGE('',*,*,#1971,.F.);
#2806=ORIENTED_EDGE('',*,*,#1874,.T.);
#2807=ORIENTED_EDGE('',*,*,#2000,.T.);
#2808=ORIENTED_EDGE('',*,*,#1868,.T.);
#2809=ORIENTED_EDGE('',*,*,#1972,.F.);
#2810=ORIENTED_EDGE('',*,*,#1870,.T.);
#2811=ORIENTED_EDGE('',*,*,#2001,.T.);
#2812=ORIENTED_EDGE('',*,*,#1864,.T.);
#2813=ORIENTED_EDGE('',*,*,#1973,.F.);
#2814=ORIENTED_EDGE('',*,*,#1866,.T.);
#2815=ORIENTED_EDGE('',*,*,#2002,.T.);
#2816=ORIENTED_EDGE('',*,*,#1860,.T.);
#2817=ORIENTED_EDGE('',*,*,#1974,.F.);
#2818=ORIENTED_EDGE('',*,*,#1862,.T.);
#2819=ORIENTED_EDGE('',*,*,#2003,.T.);
#2820=ORIENTED_EDGE('',*,*,#2004,.F.);
#2821=ORIENTED_EDGE('',*,*,#1980,.F.);
#2822=ORIENTED_EDGE('',*,*,#1951,.F.);
#2823=ORIENTED_EDGE('',*,*,#1977,.F.);
#2824=ORIENTED_EDGE('',*,*,#1979,.F.);
#2825=ORIENTED_EDGE('',*,*,#2005,.F.);
#2826=ORIENTED_EDGE('',*,*,#2006,.F.);
#2827=ORIENTED_EDGE('',*,*,#2007,.T.);
#2828=ORIENTED_EDGE('',*,*,#1949,.T.);
#2829=ORIENTED_EDGE('',*,*,#2007,.F.);
#2830=ORIENTED_EDGE('',*,*,#2006,.T.);
#2831=ORIENTED_EDGE('',*,*,#2008,.F.);
#2832=ORIENTED_EDGE('',*,*,#2009,.F.);
#2833=ORIENTED_EDGE('',*,*,#2010,.T.);
#2834=ORIENTED_EDGE('',*,*,#2008,.T.);
#2835=ORIENTED_EDGE('',*,*,#2010,.F.);
#2836=ORIENTED_EDGE('',*,*,#1853,.T.);
#2837=ORIENTED_EDGE('',*,*,#2011,.F.);
#2838=ORIENTED_EDGE('',*,*,#1857,.T.);
#2839=ORIENTED_EDGE('',*,*,#2003,.F.);
#2840=ORIENTED_EDGE('',*,*,#1861,.T.);
#2841=ORIENTED_EDGE('',*,*,#2002,.F.);
#2842=ORIENTED_EDGE('',*,*,#1865,.T.);
#2843=ORIENTED_EDGE('',*,*,#2001,.F.);
#2844=ORIENTED_EDGE('',*,*,#1869,.T.);
#2845=ORIENTED_EDGE('',*,*,#2000,.F.);
#2846=ORIENTED_EDGE('',*,*,#1873,.T.);
#2847=ORIENTED_EDGE('',*,*,#1999,.F.);
#2848=ORIENTED_EDGE('',*,*,#1877,.T.);
#2849=ORIENTED_EDGE('',*,*,#1998,.F.);
#2850=ORIENTED_EDGE('',*,*,#1881,.T.);
#2851=ORIENTED_EDGE('',*,*,#1997,.F.);
#2852=ORIENTED_EDGE('',*,*,#1885,.T.);
#2853=ORIENTED_EDGE('',*,*,#1996,.F.);
#2854=ORIENTED_EDGE('',*,*,#1889,.T.);
#2855=ORIENTED_EDGE('',*,*,#1995,.F.);
#2856=ORIENTED_EDGE('',*,*,#1893,.T.);
#2857=ORIENTED_EDGE('',*,*,#1994,.F.);
#2858=ORIENTED_EDGE('',*,*,#1897,.T.);
#2859=ORIENTED_EDGE('',*,*,#1993,.F.);
#2860=ORIENTED_EDGE('',*,*,#1901,.T.);
#2861=ORIENTED_EDGE('',*,*,#1992,.F.);
#2862=ORIENTED_EDGE('',*,*,#1905,.T.);
#2863=ORIENTED_EDGE('',*,*,#1991,.F.);
#2864=ORIENTED_EDGE('',*,*,#1909,.T.);
#2865=ORIENTED_EDGE('',*,*,#1990,.F.);
#2866=ORIENTED_EDGE('',*,*,#1913,.T.);
#2867=ORIENTED_EDGE('',*,*,#1989,.F.);
#2868=ORIENTED_EDGE('',*,*,#1917,.T.);
#2869=ORIENTED_EDGE('',*,*,#1988,.F.);
#2870=ORIENTED_EDGE('',*,*,#1921,.T.);
#2871=ORIENTED_EDGE('',*,*,#1987,.F.);
#2872=ORIENTED_EDGE('',*,*,#1925,.T.);
#2873=ORIENTED_EDGE('',*,*,#1986,.F.);
#2874=ORIENTED_EDGE('',*,*,#1929,.T.);
#2875=ORIENTED_EDGE('',*,*,#1985,.F.);
#2876=ORIENTED_EDGE('',*,*,#1933,.T.);
#2877=ORIENTED_EDGE('',*,*,#1984,.F.);
#2878=ORIENTED_EDGE('',*,*,#1937,.T.);
#2879=ORIENTED_EDGE('',*,*,#1983,.F.);
#2880=ORIENTED_EDGE('',*,*,#1941,.T.);
#2881=ORIENTED_EDGE('',*,*,#1982,.F.);
#2882=ORIENTED_EDGE('',*,*,#1945,.T.);
#2883=ORIENTED_EDGE('',*,*,#1981,.F.);
#2884=ORIENTED_EDGE('',*,*,#2004,.T.);
#2885=ORIENTED_EDGE('',*,*,#2012,.T.);
#2886=ORIENTED_EDGE('',*,*,#2009,.T.);
#2887=ORIENTED_EDGE('',*,*,#2012,.F.);
#2888=ORIENTED_EDGE('',*,*,#2005,.T.);
#2889=ORIENTED_EDGE('',*,*,#1978,.F.);
#2890=ORIENTED_EDGE('',*,*,#1856,.T.);
#2891=ORIENTED_EDGE('',*,*,#1975,.F.);
#2892=ORIENTED_EDGE('',*,*,#1858,.T.);
#2893=ORIENTED_EDGE('',*,*,#2011,.T.);
#2894=ORIENTED_EDGE('',*,*,#2013,.T.);
#2895=ORIENTED_EDGE('',*,*,#2014,.T.);
#2896=ORIENTED_EDGE('',*,*,#2015,.T.);
#2897=ORIENTED_EDGE('',*,*,#2016,.F.);
#2898=ORIENTED_EDGE('',*,*,#2017,.F.);
#2899=ORIENTED_EDGE('',*,*,#2015,.F.);
#2900=ORIENTED_EDGE('',*,*,#2018,.F.);
#2901=ORIENTED_EDGE('',*,*,#2019,.F.);
#2902=ORIENTED_EDGE('',*,*,#2020,.F.);
#2903=ORIENTED_EDGE('',*,*,#2021,.F.);
#2904=ORIENTED_EDGE('',*,*,#2020,.T.);
#2905=ORIENTED_EDGE('',*,*,#2022,.T.);
#2906=ORIENTED_EDGE('',*,*,#2023,.F.);
#2907=ORIENTED_EDGE('',*,*,#2024,.F.);
#2908=ORIENTED_EDGE('',*,*,#2019,.T.);
#2909=ORIENTED_EDGE('',*,*,#2025,.T.);
#2910=ORIENTED_EDGE('',*,*,#2026,.F.);
#2911=ORIENTED_EDGE('',*,*,#2027,.F.);
#2912=ORIENTED_EDGE('',*,*,#2022,.F.);
#2913=ORIENTED_EDGE('',*,*,#2028,.F.);
#2914=ORIENTED_EDGE('',*,*,#2029,.F.);
#2915=ORIENTED_EDGE('',*,*,#2030,.T.);
#2916=ORIENTED_EDGE('',*,*,#2031,.T.);
#2917=ORIENTED_EDGE('',*,*,#2030,.F.);
#2918=ORIENTED_EDGE('',*,*,#2032,.F.);
#2919=ORIENTED_EDGE('',*,*,#2031,.F.);
#2920=ORIENTED_EDGE('',*,*,#2018,.T.);
#2921=ORIENTED_EDGE('',*,*,#2033,.T.);
#2922=ORIENTED_EDGE('',*,*,#2034,.F.);
#2923=ORIENTED_EDGE('',*,*,#2025,.F.);
#2924=ORIENTED_EDGE('',*,*,#2021,.T.);
#2925=ORIENTED_EDGE('',*,*,#2024,.T.);
#2926=ORIENTED_EDGE('',*,*,#2035,.F.);
#2927=ORIENTED_EDGE('',*,*,#2036,.F.);
#2928=ORIENTED_EDGE('',*,*,#2033,.F.);
#2929=ORIENTED_EDGE('',*,*,#2037,.T.);
#2930=ORIENTED_EDGE('',*,*,#2038,.T.);
#2931=ORIENTED_EDGE('',*,*,#2039,.T.);
#2932=ORIENTED_EDGE('',*,*,#2040,.T.);
#2933=ORIENTED_EDGE('',*,*,#2039,.F.);
#2934=ORIENTED_EDGE('',*,*,#2040,.F.);
#2935=ORIENTED_EDGE('',*,*,#2041,.T.);
#2936=ORIENTED_EDGE('',*,*,#2042,.F.);
#2937=ORIENTED_EDGE('',*,*,#2043,.T.);
#2938=ORIENTED_EDGE('',*,*,#2037,.F.);
#2939=ORIENTED_EDGE('',*,*,#2038,.F.);
#2940=ORIENTED_EDGE('',*,*,#2043,.F.);
#2941=ORIENTED_EDGE('',*,*,#2044,.T.);
#2942=ORIENTED_EDGE('',*,*,#2045,.T.);
#2943=ORIENTED_EDGE('',*,*,#2046,.T.);
#2944=ORIENTED_EDGE('',*,*,#2045,.F.);
#2945=ORIENTED_EDGE('',*,*,#2046,.F.);
#2946=ORIENTED_EDGE('',*,*,#2047,.T.);
#2947=ORIENTED_EDGE('',*,*,#2026,.T.);
#2948=ORIENTED_EDGE('',*,*,#2034,.T.);
#2949=ORIENTED_EDGE('',*,*,#2036,.T.);
#2950=ORIENTED_EDGE('',*,*,#2048,.T.);
#2951=ORIENTED_EDGE('',*,*,#2032,.T.);
#2952=ORIENTED_EDGE('',*,*,#2049,.T.);
#2953=ORIENTED_EDGE('',*,*,#2050,.F.);
#2954=ORIENTED_EDGE('',*,*,#2049,.F.);
#2955=ORIENTED_EDGE('',*,*,#2029,.T.);
#2956=ORIENTED_EDGE('',*,*,#2028,.T.);
#2957=ORIENTED_EDGE('',*,*,#2048,.F.);
#2958=ORIENTED_EDGE('',*,*,#2035,.T.);
#2959=ORIENTED_EDGE('',*,*,#2023,.T.);
#2960=ORIENTED_EDGE('',*,*,#2027,.T.);
#2961=ORIENTED_EDGE('',*,*,#2047,.F.);
#2962=ORIENTED_EDGE('',*,*,#2044,.F.);
#2963=ORIENTED_EDGE('',*,*,#2014,.F.);
#2964=ORIENTED_EDGE('',*,*,#2013,.F.);
#2965=ORIENTED_EDGE('',*,*,#2050,.T.);
#2966=ORIENTED_EDGE('',*,*,#2051,.T.);
#2967=ORIENTED_EDGE('',*,*,#2052,.T.);
#2968=ORIENTED_EDGE('',*,*,#2051,.F.);
#2969=ORIENTED_EDGE('',*,*,#2052,.F.);
#2970=ORIENTED_EDGE('',*,*,#2042,.T.);
#2971=ORIENTED_EDGE('',*,*,#2016,.T.);
#2972=ORIENTED_EDGE('',*,*,#2017,.T.);
#2973=ORIENTED_EDGE('',*,*,#2053,.F.);
#2974=ORIENTED_EDGE('',*,*,#2053,.T.);
#2975=ORIENTED_EDGE('',*,*,#2054,.T.);
#2976=ORIENTED_EDGE('',*,*,#2041,.F.);
#2977=ORIENTED_EDGE('',*,*,#2054,.F.);
#2978=ORIENTED_EDGE('',*,*,#2055,.F.);
#2979=ORIENTED_EDGE('',*,*,#2056,.T.);
#2980=ORIENTED_EDGE('',*,*,#2056,.F.);
#2981=ORIENTED_EDGE('',*,*,#2057,.F.);
#2982=ORIENTED_EDGE('',*,*,#2058,.F.);
#2983=ORIENTED_EDGE('',*,*,#2058,.T.);
#2984=ORIENTED_EDGE('',*,*,#2059,.F.);
#2985=ORIENTED_EDGE('',*,*,#2055,.T.);
#2986=ORIENTED_EDGE('',*,*,#2057,.T.);
#2987=ORIENTED_EDGE('',*,*,#2060,.T.);
#2988=ORIENTED_EDGE('',*,*,#2060,.F.);
#2989=ORIENTED_EDGE('',*,*,#2061,.T.);
#2990=ORIENTED_EDGE('',*,*,#2059,.T.);
#2991=ORIENTED_EDGE('',*,*,#2061,.F.);
#2992=ORIENTED_EDGE('',*,*,#2062,.T.);
#2993=ORIENTED_EDGE('',*,*,#2063,.T.);
#2994=ORIENTED_EDGE('',*,*,#2064,.T.);
#2995=ORIENTED_EDGE('',*,*,#2063,.F.);
#2996=ORIENTED_EDGE('',*,*,#2062,.F.);
#2997=ORIENTED_EDGE('',*,*,#2065,.T.);
#2998=ORIENTED_EDGE('',*,*,#2066,.F.);
#2999=ORIENTED_EDGE('',*,*,#2067,.T.);
#3000=ORIENTED_EDGE('',*,*,#2064,.F.);
#3001=ORIENTED_EDGE('',*,*,#2067,.F.);
#3002=ORIENTED_EDGE('',*,*,#2068,.F.);
#3003=ORIENTED_EDGE('',*,*,#2065,.F.);
#3004=ORIENTED_EDGE('',*,*,#2069,.T.);
#3005=ORIENTED_EDGE('',*,*,#2068,.T.);
#3006=ORIENTED_EDGE('',*,*,#2069,.F.);
#3007=ORIENTED_EDGE('',*,*,#2066,.T.);
#3008=ORIENTED_EDGE('',*,*,#2070,.T.);
#3009=ORIENTED_EDGE('',*,*,#2070,.F.);
#3010=ORIENTED_EDGE('',*,*,#2071,.F.);
#3011=ORIENTED_EDGE('',*,*,#2072,.T.);
#3012=ORIENTED_EDGE('',*,*,#2073,.T.);
#3013=ORIENTED_EDGE('',*,*,#2072,.F.);
#3014=ORIENTED_EDGE('',*,*,#2071,.T.);
#3015=ORIENTED_EDGE('',*,*,#2073,.F.);
#3016=ORIENTED_EDGE('',*,*,#2074,.F.);
#3017=ORIENTED_EDGE('',*,*,#2075,.T.);
#3018=ORIENTED_EDGE('',*,*,#2076,.T.);
#3019=ORIENTED_EDGE('',*,*,#2075,.F.);
#3020=ORIENTED_EDGE('',*,*,#2077,.F.);
#3021=ORIENTED_EDGE('',*,*,#2078,.T.);
#3022=ORIENTED_EDGE('',*,*,#2079,.T.);
#3023=ORIENTED_EDGE('',*,*,#2078,.F.);
#3024=ORIENTED_EDGE('',*,*,#2077,.T.);
#3025=ORIENTED_EDGE('',*,*,#2074,.T.);
#3026=ORIENTED_EDGE('',*,*,#2079,.F.);
#3027=ORIENTED_EDGE('',*,*,#2076,.F.);
#3028=TOROIDAL_SURFACE('',#3337,10.0057959473896,0.5);
#3029=TOROIDAL_SURFACE('',#3517,1.5,0.5);
#3030=TOROIDAL_SURFACE('',#3659,10.5246348408465,0.5);
#3031=TOROIDAL_SURFACE('',#3666,10.5246348408465,0.5);
#3032=ADVANCED_FACE('',(#728),#3028,.T.);
#3033=ADVANCED_FACE('',(#729,#689),#700,.T.);
#3034=ADVANCED_FACE('',(#730),#549,.T.);
#3035=ADVANCED_FACE('',(#731),#550,.F.);
#3036=ADVANCED_FACE('',(#732),#551,.F.);
#3037=ADVANCED_FACE('',(#733),#552,.F.);
#3038=ADVANCED_FACE('',(#734),#553,.F.);
#3039=ADVANCED_FACE('',(#735),#554,.F.);
#3040=ADVANCED_FACE('',(#736),#555,.F.);
#3041=ADVANCED_FACE('',(#737),#556,.F.);
#3042=ADVANCED_FACE('',(#738),#557,.F.);
#3043=ADVANCED_FACE('',(#739),#558,.F.);
#3044=ADVANCED_FACE('',(#740),#559,.F.);
#3045=ADVANCED_FACE('',(#741),#560,.F.);
#3046=ADVANCED_FACE('',(#742),#561,.F.);
#3047=ADVANCED_FACE('',(#743),#562,.F.);
#3048=ADVANCED_FACE('',(#744),#563,.F.);
#3049=ADVANCED_FACE('',(#745),#564,.F.);
#3050=ADVANCED_FACE('',(#746),#565,.F.);
#3051=ADVANCED_FACE('',(#747),#566,.F.);
#3052=ADVANCED_FACE('',(#748),#567,.F.);
#3053=ADVANCED_FACE('',(#749),#568,.F.);
#3054=ADVANCED_FACE('',(#750),#569,.F.);
#3055=ADVANCED_FACE('',(#751),#570,.F.);
#3056=ADVANCED_FACE('',(#752),#571,.F.);
#3057=ADVANCED_FACE('',(#753),#572,.F.);
#3058=ADVANCED_FACE('',(#754),#573,.F.);
#3059=ADVANCED_FACE('',(#755),#97,.T.);
#3060=ADVANCED_FACE('',(#756),#574,.T.);
#3061=ADVANCED_FACE('',(#757),#575,.T.);
#3062=ADVANCED_FACE('',(#758),#576,.T.);
#3063=ADVANCED_FACE('',(#759),#577,.T.);
#3064=ADVANCED_FACE('',(#760),#578,.T.);
#3065=ADVANCED_FACE('',(#761),#579,.T.);
#3066=ADVANCED_FACE('',(#762),#580,.T.);
#3067=ADVANCED_FACE('',(#763),#581,.T.);
#3068=ADVANCED_FACE('',(#764),#582,.T.);
#3069=ADVANCED_FACE('',(#765),#583,.T.);
#3070=ADVANCED_FACE('',(#766),#584,.T.);
#3071=ADVANCED_FACE('',(#767),#585,.T.);
#3072=ADVANCED_FACE('',(#768),#586,.T.);
#3073=ADVANCED_FACE('',(#769),#587,.T.);
#3074=ADVANCED_FACE('',(#770),#588,.T.);
#3075=ADVANCED_FACE('',(#771),#589,.T.);
#3076=ADVANCED_FACE('',(#772),#590,.T.);
#3077=ADVANCED_FACE('',(#773),#591,.T.);
#3078=ADVANCED_FACE('',(#774),#592,.T.);
#3079=ADVANCED_FACE('',(#775),#593,.T.);
#3080=ADVANCED_FACE('',(#776),#594,.T.);
#3081=ADVANCED_FACE('',(#777),#595,.T.);
#3082=ADVANCED_FACE('',(#778),#596,.T.);
#3083=ADVANCED_FACE('',(#779),#597,.T.);
#3084=ADVANCED_FACE('',(#780),#598,.F.);
#3085=ADVANCED_FACE('',(#781),#98,.T.);
#3086=ADVANCED_FACE('',(#782),#599,.T.);
#3087=ADVANCED_FACE('',(#783),#701,.T.);
#3088=ADVANCED_FACE('',(#784),#702,.T.);
#3089=ADVANCED_FACE('',(#785),#600,.F.);
#3090=ADVANCED_FACE('',(#786),#99,.T.);
#3091=ADVANCED_FACE('',(#787),#703,.F.);
#3092=ADVANCED_FACE('',(#788),#704,.T.);
#3093=ADVANCED_FACE('',(#789),#100,.T.);
#3094=ADVANCED_FACE('',(#790),#601,.T.);
#3095=ADVANCED_FACE('',(#791),#705,.T.);
#3096=ADVANCED_FACE('',(#792),#602,.F.);
#3097=ADVANCED_FACE('',(#793),#706,.T.);
#3098=ADVANCED_FACE('',(#794),#603,.F.);
#3099=ADVANCED_FACE('',(#795),#604,.F.);
#3100=ADVANCED_FACE('',(#796),#605,.F.);
#3101=ADVANCED_FACE('',(#797),#606,.F.);
#3102=ADVANCED_FACE('',(#798),#607,.F.);
#3103=ADVANCED_FACE('',(#799),#608,.F.);
#3104=ADVANCED_FACE('',(#800),#609,.F.);
#3105=ADVANCED_FACE('',(#801),#610,.F.);
#3106=ADVANCED_FACE('',(#802),#611,.F.);
#3107=ADVANCED_FACE('',(#803,#690),#707,.F.);
#3108=ADVANCED_FACE('',(#804),#612,.T.);
#3109=ADVANCED_FACE('',(#805),#613,.T.);
#3110=ADVANCED_FACE('',(#806),#614,.T.);
#3111=ADVANCED_FACE('',(#807),#615,.T.);
#3112=ADVANCED_FACE('',(#808),#616,.T.);
#3113=ADVANCED_FACE('',(#809),#617,.T.);
#3114=ADVANCED_FACE('',(#810),#618,.T.);
#3115=ADVANCED_FACE('',(#811),#619,.T.);
#3116=ADVANCED_FACE('',(#812),#620,.T.);
#3117=ADVANCED_FACE('',(#813),#3029,.T.);
#3118=ADVANCED_FACE('',(#814),#621,.F.);
#3119=ADVANCED_FACE('',(#815),#622,.T.);
#3120=ADVANCED_FACE('',(#816),#708,.T.);
#3121=ADVANCED_FACE('',(#817),#623,.T.);
#3122=ADVANCED_FACE('',(#818),#709,.F.);
#3123=ADVANCED_FACE('',(#819),#624,.F.);
#3124=ADVANCED_FACE('',(#820),#625,.F.);
#3125=ADVANCED_FACE('',(#821),#626,.F.);
#3126=ADVANCED_FACE('',(#822),#627,.F.);
#3127=ADVANCED_FACE('',(#823),#628,.F.);
#3128=ADVANCED_FACE('',(#824),#629,.F.);
#3129=ADVANCED_FACE('',(#825),#630,.F.);
#3130=ADVANCED_FACE('',(#826),#631,.F.);
#3131=ADVANCED_FACE('',(#827),#632,.F.);
#3132=ADVANCED_FACE('',(#828),#633,.F.);
#3133=ADVANCED_FACE('',(#829),#634,.F.);
#3134=ADVANCED_FACE('',(#830),#635,.F.);
#3135=ADVANCED_FACE('',(#831),#636,.F.);
#3136=ADVANCED_FACE('',(#832),#637,.F.);
#3137=ADVANCED_FACE('',(#833),#638,.F.);
#3138=ADVANCED_FACE('',(#834),#639,.F.);
#3139=ADVANCED_FACE('',(#835),#640,.F.);
#3140=ADVANCED_FACE('',(#836),#641,.F.);
#3141=ADVANCED_FACE('',(#837),#642,.F.);
#3142=ADVANCED_FACE('',(#838),#643,.F.);
#3143=ADVANCED_FACE('',(#839),#644,.F.);
#3144=ADVANCED_FACE('',(#840),#645,.F.);
#3145=ADVANCED_FACE('',(#841),#646,.F.);
#3146=ADVANCED_FACE('',(#842),#647,.F.);
#3147=ADVANCED_FACE('',(#843),#101,.T.);
#3148=ADVANCED_FACE('',(#844),#648,.T.);
#3149=ADVANCED_FACE('',(#845),#649,.T.);
#3150=ADVANCED_FACE('',(#846),#650,.T.);
#3151=ADVANCED_FACE('',(#847),#651,.T.);
#3152=ADVANCED_FACE('',(#848),#652,.T.);
#3153=ADVANCED_FACE('',(#849),#653,.T.);
#3154=ADVANCED_FACE('',(#850),#654,.T.);
#3155=ADVANCED_FACE('',(#851),#655,.T.);
#3156=ADVANCED_FACE('',(#852),#656,.T.);
#3157=ADVANCED_FACE('',(#853),#657,.T.);
#3158=ADVANCED_FACE('',(#854),#658,.T.);
#3159=ADVANCED_FACE('',(#855),#659,.T.);
#3160=ADVANCED_FACE('',(#856),#660,.T.);
#3161=ADVANCED_FACE('',(#857),#661,.T.);
#3162=ADVANCED_FACE('',(#858),#662,.T.);
#3163=ADVANCED_FACE('',(#859),#663,.T.);
#3164=ADVANCED_FACE('',(#860),#664,.T.);
#3165=ADVANCED_FACE('',(#861),#665,.T.);
#3166=ADVANCED_FACE('',(#862),#666,.T.);
#3167=ADVANCED_FACE('',(#863),#667,.T.);
#3168=ADVANCED_FACE('',(#864),#668,.T.);
#3169=ADVANCED_FACE('',(#865),#669,.T.);
#3170=ADVANCED_FACE('',(#866),#670,.T.);
#3171=ADVANCED_FACE('',(#867),#671,.T.);
#3172=ADVANCED_FACE('',(#868),#672,.F.);
#3173=ADVANCED_FACE('',(#869),#673,.T.);
#3174=ADVANCED_FACE('',(#870),#710,.T.);
#3175=ADVANCED_FACE('',(#871),#711,.T.);
#3176=ADVANCED_FACE('',(#872),#674,.T.);
#3177=ADVANCED_FACE('',(#873),#102,.T.);
#3178=ADVANCED_FACE('',(#874),#675,.T.);
#3179=ADVANCED_FACE('',(#875,#691),#676,.F.);
#3180=ADVANCED_FACE('',(#876),#712,.F.);
#3181=ADVANCED_FACE('',(#877),#677,.F.);
#3182=ADVANCED_FACE('',(#878),#678,.F.);
#3183=ADVANCED_FACE('',(#879),#713,.T.);
#3184=ADVANCED_FACE('',(#880),#714,.F.);
#3185=ADVANCED_FACE('',(#881),#679,.F.);
#3186=ADVANCED_FACE('',(#882),#103,.T.);
#3187=ADVANCED_FACE('',(#883,#692),#715,.T.);
#3188=ADVANCED_FACE('',(#884),#680,.T.);
#3189=ADVANCED_FACE('',(#885),#3030,.T.);
#3190=ADVANCED_FACE('',(#886),#681,.T.);
#3191=ADVANCED_FACE('',(#887,#693),#716,.T.);
#3192=ADVANCED_FACE('',(#888),#3031,.T.);
#3193=ADVANCED_FACE('',(#889,#694),#717,.T.);
#3194=ADVANCED_FACE('',(#890,#695),#718,.T.);
#3195=ADVANCED_FACE('',(#891),#682,.F.);
#3196=ADVANCED_FACE('',(#892),#51,.F.);
#3197=ADVANCED_FACE('',(#893,#696),#719,.F.);
#3198=ADVANCED_FACE('',(#894),#720,.T.);
#3199=ADVANCED_FACE('',(#895),#683,.T.);
#3200=ADVANCED_FACE('',(#896),#104,.T.);
#3201=ADVANCED_FACE('',(#897,#697),#721,.T.);
#3202=ADVANCED_FACE('',(#898),#684,.T.);
#3203=ADVANCED_FACE('',(#899),#722,.F.);
#3204=ADVANCED_FACE('',(#900),#685,.F.);
#3205=ADVANCED_FACE('',(#901),#723,.F.);
#3206=ADVANCED_FACE('',(#902),#52,.T.);
#3207=ADVANCED_FACE('',(#903),#686,.T.);
#3208=ADVANCED_FACE('',(#904),#724,.T.);
#3209=ADVANCED_FACE('',(#905),#725,.F.);
#3210=ADVANCED_FACE('',(#906),#687,.F.);
#3211=ADVANCED_FACE('',(#907),#688,.T.);
#3212=ADVANCED_FACE('',(#908,#698),#726,.T.);
#3213=ADVANCED_FACE('',(#909,#699),#727,.F.);
#3214=CLOSED_SHELL('',(#3032,#3033,#3034,#3035,#3036,#3037,#3038,#3039,
#3040,#3041,#3042,#3043,#3044,#3045,#3046,#3047,#3048,#3049,#3050,#3051,
#3052,#3053,#3054,#3055,#3056,#3057,#3058,#3059,#3060,#3061,#3062,#3063,
#3064,#3065,#3066,#3067,#3068,#3069,#3070,#3071,#3072,#3073,#3074,#3075,
#3076,#3077,#3078,#3079,#3080,#3081,#3082,#3083,#3084,#3085,#3086,#3087,
#3088,#3089));
#3215=CLOSED_SHELL('',(#3090,#3091,#3092,#3093,#3094,#3095,#3096,#3097));
#3216=CLOSED_SHELL('',(#3098,#3099,#3100,#3101,#3102,#3103,#3104,#3105,
#3106,#3107,#3108,#3109,#3110,#3111,#3112,#3113,#3114,#3115,#3116,#3117,
#3118,#3119,#3120,#3121,#3122));
#3217=CLOSED_SHELL('',(#3123,#3124,#3125,#3126,#3127,#3128,#3129,#3130,
#3131,#3132,#3133,#3134,#3135,#3136,#3137,#3138,#3139,#3140,#3141,#3142,
#3143,#3144,#3145,#3146,#3147,#3148,#3149,#3150,#3151,#3152,#3153,#3154,
#3155,#3156,#3157,#3158,#3159,#3160,#3161,#3162,#3163,#3164,#3165,#3166,
#3167,#3168,#3169,#3170,#3171,#3172,#3173,#3174,#3175,#3176,#3177,#3178));
#3218=CLOSED_SHELL('',(#3179,#3180,#3181,#3182,#3183,#3184,#3185,#3186,
#3187,#3188,#3189,#3190,#3191,#3192,#3193,#3194,#3195));
#3219=CLOSED_SHELL('',(#3196,#3197,#3198,#3199));
#3220=CLOSED_SHELL('',(#3200,#3201,#3202,#3203,#3204,#3205));
#3221=CLOSED_SHELL('',(#3206));
#3222=CLOSED_SHELL('',(#3207,#3208,#3209));
#3223=CLOSED_SHELL('',(#3210,#3211,#3212,#3213));
#3224=DERIVED_UNIT_ELEMENT(#3244,1.);
#3225=DERIVED_UNIT_ELEMENT(#7317,-3.);
#3226=DERIVED_UNIT_ELEMENT(#3244,1.);
#3227=DERIVED_UNIT_ELEMENT(#7317,-3.);
#3228=DERIVED_UNIT_ELEMENT(#3244,1.);
#3229=DERIVED_UNIT_ELEMENT(#7317,-3.);
#3230=DERIVED_UNIT_ELEMENT(#3244,1.);
#3231=DERIVED_UNIT_ELEMENT(#7317,-3.);
#3232=DERIVED_UNIT_ELEMENT(#3244,1.);
#3233=DERIVED_UNIT_ELEMENT(#7317,-3.);
#3234=DERIVED_UNIT_ELEMENT(#3244,1.);
#3235=DERIVED_UNIT_ELEMENT(#7317,-3.);
#3236=DERIVED_UNIT_ELEMENT(#3244,1.);
#3237=DERIVED_UNIT_ELEMENT(#7317,-3.);
#3238=DERIVED_UNIT_ELEMENT(#3244,1.);
#3239=DERIVED_UNIT_ELEMENT(#7317,-3.);
#3240=DERIVED_UNIT_ELEMENT(#3244,1.);
#3241=DERIVED_UNIT_ELEMENT(#7317,-3.);
#3242=DERIVED_UNIT_ELEMENT(#3244,1.);
#3243=DERIVED_UNIT_ELEMENT(#7317,-3.);
#3244=(
MASS_UNIT()
NAMED_UNIT(*)
SI_UNIT(.KILO.,.GRAM.)
);
#3245=DERIVED_UNIT((#3224,#3225));
#3246=DERIVED_UNIT((#3226,#3227));
#3247=DERIVED_UNIT((#3228,#3229));
#3248=DERIVED_UNIT((#3230,#3231));
#3249=DERIVED_UNIT((#3232,#3233));
#3250=DERIVED_UNIT((#3234,#3235));
#3251=DERIVED_UNIT((#3236,#3237));
#3252=DERIVED_UNIT((#3238,#3239));
#3253=DERIVED_UNIT((#3240,#3241));
#3254=DERIVED_UNIT((#3242,#3243));
#3255=MEASURE_REPRESENTATION_ITEM('density measure',
POSITIVE_RATIO_MEASURE(7850.),#3245);
#3256=MEASURE_REPRESENTATION_ITEM('density measure',
POSITIVE_RATIO_MEASURE(7850.),#3246);
#3257=MEASURE_REPRESENTATION_ITEM('density measure',
POSITIVE_RATIO_MEASURE(7850.),#3247);
#3258=MEASURE_REPRESENTATION_ITEM('density measure',
POSITIVE_RATIO_MEASURE(7850.),#3248);
#3259=MEASURE_REPRESENTATION_ITEM('density measure',
POSITIVE_RATIO_MEASURE(7850.),#3249);
#3260=MEASURE_REPRESENTATION_ITEM('density measure',
POSITIVE_RATIO_MEASURE(7850.),#3250);
#3261=MEASURE_REPRESENTATION_ITEM('density measure',
POSITIVE_RATIO_MEASURE(7850.),#3251);
#3262=MEASURE_REPRESENTATION_ITEM('density measure',
POSITIVE_RATIO_MEASURE(7850.),#3252);
#3263=MEASURE_REPRESENTATION_ITEM('density measure',
POSITIVE_RATIO_MEASURE(7850.),#3253);
#3264=MEASURE_REPRESENTATION_ITEM('density measure',
POSITIVE_RATIO_MEASURE(7850.),#3254);
#3265=PROPERTY_DEFINITION_REPRESENTATION(#3315,#3285);
#3266=PROPERTY_DEFINITION_REPRESENTATION(#3316,#3286);
#3267=PROPERTY_DEFINITION_REPRESENTATION(#3317,#3287);
#3268=PROPERTY_DEFINITION_REPRESENTATION(#3318,#3288);
#3269=PROPERTY_DEFINITION_REPRESENTATION(#3319,#3289);
#3270=PROPERTY_DEFINITION_REPRESENTATION(#3320,#3290);
#3271=PROPERTY_DEFINITION_REPRESENTATION(#3321,#3291);
#3272=PROPERTY_DEFINITION_REPRESENTATION(#3322,#3292);
#3273=PROPERTY_DEFINITION_REPRESENTATION(#3323,#3293);
#3274=PROPERTY_DEFINITION_REPRESENTATION(#3324,#3294);
#3275=PROPERTY_DEFINITION_REPRESENTATION(#3325,#3295);
#3276=PROPERTY_DEFINITION_REPRESENTATION(#3326,#3296);
#3277=PROPERTY_DEFINITION_REPRESENTATION(#3327,#3297);
#3278=PROPERTY_DEFINITION_REPRESENTATION(#3328,#3298);
#3279=PROPERTY_DEFINITION_REPRESENTATION(#3329,#3299);
#3280=PROPERTY_DEFINITION_REPRESENTATION(#3330,#3300);
#3281=PROPERTY_DEFINITION_REPRESENTATION(#3331,#3301);
#3282=PROPERTY_DEFINITION_REPRESENTATION(#3332,#3302);
#3283=PROPERTY_DEFINITION_REPRESENTATION(#3333,#3303);
#3284=PROPERTY_DEFINITION_REPRESENTATION(#3334,#3304);
#3285=REPRESENTATION('material name',(#3305),#7305);
#3286=REPRESENTATION('density',(#3255),#7305);
#3287=REPRESENTATION('material name',(#3306),#7306);
#3288=REPRESENTATION('density',(#3256),#7306);
#3289=REPRESENTATION('material name',(#3307),#7307);
#3290=REPRESENTATION('density',(#3257),#7307);
#3291=REPRESENTATION('material name',(#3308),#7308);
#3292=REPRESENTATION('density',(#3258),#7308);
#3293=REPRESENTATION('material name',(#3309),#7309);
#3294=REPRESENTATION('density',(#3259),#7309);
#3295=REPRESENTATION('material name',(#3310),#7310);
#3296=REPRESENTATION('density',(#3260),#7310);
#3297=REPRESENTATION('material name',(#3311),#7311);
#3298=REPRESENTATION('density',(#3261),#7311);
#3299=REPRESENTATION('material name',(#3312),#7312);
#3300=REPRESENTATION('density',(#3262),#7312);
#3301=REPRESENTATION('material name',(#3313),#7313);
#3302=REPRESENTATION('density',(#3263),#7313);
#3303=REPRESENTATION('material name',(#3314),#7314);
#3304=REPRESENTATION('density',(#3264),#7314);
#3305=DESCRIPTIVE_REPRESENTATION_ITEM('Steel','Steel');
#3306=DESCRIPTIVE_REPRESENTATION_ITEM('Steel','Steel');
#3307=DESCRIPTIVE_REPRESENTATION_ITEM('Steel','Steel');
#3308=DESCRIPTIVE_REPRESENTATION_ITEM('Steel','Steel');
#3309=DESCRIPTIVE_REPRESENTATION_ITEM('Steel','Steel');
#3310=DESCRIPTIVE_REPRESENTATION_ITEM('Steel','Steel');
#3311=DESCRIPTIVE_REPRESENTATION_ITEM('Steel','Steel');
#3312=DESCRIPTIVE_REPRESENTATION_ITEM('Steel','Steel');
#3313=DESCRIPTIVE_REPRESENTATION_ITEM('Steel','Steel');
#3314=DESCRIPTIVE_REPRESENTATION_ITEM('Steel','Steel');
#3315=PROPERTY_DEFINITION('material property','material name',#7365);
#3316=PROPERTY_DEFINITION('material property','density of part',#7365);
#3317=PROPERTY_DEFINITION('material property','material name',#7366);
#3318=PROPERTY_DEFINITION('material property','density of part',#7366);
#3319=PROPERTY_DEFINITION('material property','material name',#7367);
#3320=PROPERTY_DEFINITION('material property','density of part',#7367);
#3321=PROPERTY_DEFINITION('material property','material name',#7368);
#3322=PROPERTY_DEFINITION('material property','density of part',#7368);
#3323=PROPERTY_DEFINITION('material property','material name',#7369);
#3324=PROPERTY_DEFINITION('material property','density of part',#7369);
#3325=PROPERTY_DEFINITION('material property','material name',#7370);
#3326=PROPERTY_DEFINITION('material property','density of part',#7370);
#3327=PROPERTY_DEFINITION('material property','material name',#7371);
#3328=PROPERTY_DEFINITION('material property','density of part',#7371);
#3329=PROPERTY_DEFINITION('material property','material name',#7372);
#3330=PROPERTY_DEFINITION('material property','density of part',#7372);
#3331=PROPERTY_DEFINITION('material property','material name',#7373);
#3332=PROPERTY_DEFINITION('material property','density of part',#7373);
#3333=PROPERTY_DEFINITION('material property','material name',#7374);
#3334=PROPERTY_DEFINITION('material property','density of part',#7374);
#3335=AXIS2_PLACEMENT_3D('',#4662,#3724,#3725);
#3336=AXIS2_PLACEMENT_3D('',#4663,#3726,#3727);
#3337=AXIS2_PLACEMENT_3D('',#4664,#3728,#3729);
#3338=AXIS2_PLACEMENT_3D('',#4666,#3730,#3731);
#3339=AXIS2_PLACEMENT_3D('',#4668,#3732,#3733);
#3340=AXIS2_PLACEMENT_3D('',#4669,#3734,#3735);
#3341=AXIS2_PLACEMENT_3D('',#4670,#3736,#3737);
#3342=AXIS2_PLACEMENT_3D('',#4672,#3738,#3739);
#3343=AXIS2_PLACEMENT_3D('',#4673,#3740,#3741);
#3344=AXIS2_PLACEMENT_3D('',#4675,#3742,#3743);
#3345=AXIS2_PLACEMENT_3D('',#4677,#3745,#3746);
#3346=AXIS2_PLACEMENT_3D('',#4712,#3749,#3750);
#3347=AXIS2_PLACEMENT_3D('',#4747,#3753,#3754);
#3348=AXIS2_PLACEMENT_3D('',#4782,#3757,#3758);
#3349=AXIS2_PLACEMENT_3D('',#4817,#3761,#3762);
#3350=AXIS2_PLACEMENT_3D('',#4852,#3765,#3766);
#3351=AXIS2_PLACEMENT_3D('',#4887,#3769,#3770);
#3352=AXIS2_PLACEMENT_3D('',#4922,#3773,#3774);
#3353=AXIS2_PLACEMENT_3D('',#4957,#3777,#3778);
#3354=AXIS2_PLACEMENT_3D('',#4992,#3781,#3782);
#3355=AXIS2_PLACEMENT_3D('',#5027,#3785,#3786);
#3356=AXIS2_PLACEMENT_3D('',#5062,#3789,#3790);
#3357=AXIS2_PLACEMENT_3D('',#5097,#3793,#3794);
#3358=AXIS2_PLACEMENT_3D('',#5132,#3797,#3798);
#3359=AXIS2_PLACEMENT_3D('',#5167,#3801,#3802);
#3360=AXIS2_PLACEMENT_3D('',#5202,#3805,#3806);
#3361=AXIS2_PLACEMENT_3D('',#5237,#3809,#3810);
#3362=AXIS2_PLACEMENT_3D('',#5272,#3813,#3814);
#3363=AXIS2_PLACEMENT_3D('',#5307,#3817,#3818);
#3364=AXIS2_PLACEMENT_3D('',#5342,#3821,#3822);
#3365=AXIS2_PLACEMENT_3D('',#5377,#3825,#3826);
#3366=AXIS2_PLACEMENT_3D('',#5412,#3829,#3830);
#3367=AXIS2_PLACEMENT_3D('',#5447,#3833,#3834);
#3368=AXIS2_PLACEMENT_3D('',#5482,#3837,#3838);
#3369=AXIS2_PLACEMENT_3D('',#5517,#3841,#3842);
#3370=AXIS2_PLACEMENT_3D('',#5519,#3843,#3844);
#3371=AXIS2_PLACEMENT_3D('',#5531,#3846,#3847);
#3372=AXIS2_PLACEMENT_3D('',#5532,#3848,#3849);
#3373=AXIS2_PLACEMENT_3D('',#5533,#3850,#3851);
#3374=AXIS2_PLACEMENT_3D('',#5534,#3852,#3853);
#3375=AXIS2_PLACEMENT_3D('',#5535,#3854,#3855);
#3376=AXIS2_PLACEMENT_3D('',#5536,#3856,#3857);
#3377=AXIS2_PLACEMENT_3D('',#5537,#3858,#3859);
#3378=AXIS2_PLACEMENT_3D('',#5538,#3860,#3861);
#3379=AXIS2_PLACEMENT_3D('',#5539,#3862,#3863);
#3380=AXIS2_PLACEMENT_3D('',#5540,#3864,#3865);
#3381=AXIS2_PLACEMENT_3D('',#5541,#3866,#3867);
#3382=AXIS2_PLACEMENT_3D('',#5542,#3868,#3869);
#3383=AXIS2_PLACEMENT_3D('',#5543,#3870,#3871);
#3384=AXIS2_PLACEMENT_3D('',#5544,#3872,#3873);
#3385=AXIS2_PLACEMENT_3D('',#5545,#3874,#3875);
#3386=AXIS2_PLACEMENT_3D('',#5546,#3876,#3877);
#3387=AXIS2_PLACEMENT_3D('',#5547,#3878,#3879);
#3388=AXIS2_PLACEMENT_3D('',#5548,#3880,#3881);
#3389=AXIS2_PLACEMENT_3D('',#5549,#3882,#3883);
#3390=AXIS2_PLACEMENT_3D('',#5550,#3884,#3885);
#3391=AXIS2_PLACEMENT_3D('',#5551,#3886,#3887);
#3392=AXIS2_PLACEMENT_3D('',#5552,#3888,#3889);
#3393=AXIS2_PLACEMENT_3D('',#5553,#3890,#3891);
#3394=AXIS2_PLACEMENT_3D('',#5554,#3892,#3893);
#3395=AXIS2_PLACEMENT_3D('',#5556,#3894,#3895);
#3396=AXIS2_PLACEMENT_3D('',#5565,#3896,#3897);
#3397=AXIS2_PLACEMENT_3D('',#5567,#3898,#3899);
#3398=AXIS2_PLACEMENT_3D('',#5569,#3901,#3902);
#3399=AXIS2_PLACEMENT_3D('',#5572,#3904,#3905);
#3400=AXIS2_PLACEMENT_3D('',#5573,#3906,#3907);
#3401=AXIS2_PLACEMENT_3D('',#5574,#3908,#3909);
#3402=AXIS2_PLACEMENT_3D('',#5575,#3910,#3911);
#3403=AXIS2_PLACEMENT_3D('',#5576,#3912,#3913);
#3404=AXIS2_PLACEMENT_3D('',#5577,#3914,#3915);
#3405=AXIS2_PLACEMENT_3D('',#5578,#3916,#3917);
#3406=AXIS2_PLACEMENT_3D('',#5579,#3918,#3919);
#3407=AXIS2_PLACEMENT_3D('',#5580,#3920,#3921);
#3408=AXIS2_PLACEMENT_3D('',#5581,#3922,#3923);
#3409=AXIS2_PLACEMENT_3D('',#5582,#3924,#3925);
#3410=AXIS2_PLACEMENT_3D('',#5583,#3926,#3927);
#3411=AXIS2_PLACEMENT_3D('',#5584,#3928,#3929);
#3412=AXIS2_PLACEMENT_3D('',#5585,#3930,#3931);
#3413=AXIS2_PLACEMENT_3D('',#5586,#3932,#3933);
#3414=AXIS2_PLACEMENT_3D('',#5587,#3934,#3935);
#3415=AXIS2_PLACEMENT_3D('',#5588,#3936,#3937);
#3416=AXIS2_PLACEMENT_3D('',#5589,#3938,#3939);
#3417=AXIS2_PLACEMENT_3D('',#5590,#3940,#3941);
#3418=AXIS2_PLACEMENT_3D('',#5591,#3942,#3943);
#3419=AXIS2_PLACEMENT_3D('',#5592,#3944,#3945);
#3420=AXIS2_PLACEMENT_3D('',#5593,#3946,#3947);
#3421=AXIS2_PLACEMENT_3D('',#5594,#3948,#3949);
#3422=AXIS2_PLACEMENT_3D('',#5595,#3950,#3951);
#3423=AXIS2_PLACEMENT_3D('',#5596,#3952,#3953);
#3424=AXIS2_PLACEMENT_3D('',#5597,#3954,#3955);
#3425=AXIS2_PLACEMENT_3D('',#5598,#3956,#3957);
#3426=AXIS2_PLACEMENT_3D('',#5599,#3958,#3959);
#3427=AXIS2_PLACEMENT_3D('',#5600,#3960,#3961);
#3428=AXIS2_PLACEMENT_3D('',#5601,#3962,#3963);
#3429=AXIS2_PLACEMENT_3D('',#5602,#3964,#3965);
#3430=AXIS2_PLACEMENT_3D('',#5603,#3966,#3967);
#3431=AXIS2_PLACEMENT_3D('',#5604,#3968,#3969);
#3432=AXIS2_PLACEMENT_3D('',#5605,#3970,#3971);
#3433=AXIS2_PLACEMENT_3D('',#5606,#3972,#3973);
#3434=AXIS2_PLACEMENT_3D('',#5607,#3974,#3975);
#3435=AXIS2_PLACEMENT_3D('',#5608,#3976,#3977);
#3436=AXIS2_PLACEMENT_3D('',#5609,#3978,#3979);
#3437=AXIS2_PLACEMENT_3D('',#5610,#3980,#3981);
#3438=AXIS2_PLACEMENT_3D('',#5611,#3982,#3983);
#3439=AXIS2_PLACEMENT_3D('',#5612,#3984,#3985);
#3440=AXIS2_PLACEMENT_3D('',#5613,#3986,#3987);
#3441=AXIS2_PLACEMENT_3D('',#5614,#3988,#3989);
#3442=AXIS2_PLACEMENT_3D('',#5615,#3990,#3991);
#3443=AXIS2_PLACEMENT_3D('',#5616,#3992,#3993);
#3444=AXIS2_PLACEMENT_3D('',#5617,#3994,#3995);
#3445=AXIS2_PLACEMENT_3D('',#5635,#3996,#3997);
#3446=AXIS2_PLACEMENT_3D('',#5636,#3998,#3999);
#3447=AXIS2_PLACEMENT_3D('',#5638,#4001,#4002);
#3448=AXIS2_PLACEMENT_3D('',#5639,#4003,#4004);
#3449=AXIS2_PLACEMENT_3D('',#5640,#4005,#4006);
#3450=AXIS2_PLACEMENT_3D('',#5642,#4007,#4008);
#3451=AXIS2_PLACEMENT_3D('',#5643,#4009,#4010);
#3452=AXIS2_PLACEMENT_3D('',#5645,#4012,#4013);
#3453=AXIS2_PLACEMENT_3D('',#5646,#4014,#4015);
#3454=AXIS2_PLACEMENT_3D('',#5653,#4016,#4017);
#3455=AXIS2_PLACEMENT_3D('',#5658,#4018,#4019);
#3456=AXIS2_PLACEMENT_3D('',#5659,#4020,#4021);
#3457=AXIS2_PLACEMENT_3D('',#5663,#4023,#4024);
#3458=AXIS2_PLACEMENT_3D('',#5665,#4026,#4027);
#3459=AXIS2_PLACEMENT_3D('',#5675,#4031,#4032);
#3460=AXIS2_PLACEMENT_3D('',#5681,#4033,#4034);
#3461=AXIS2_PLACEMENT_3D('',#5682,#4035,#4036);
#3462=AXIS2_PLACEMENT_3D('',#5683,#4037,#4038);
#3463=AXIS2_PLACEMENT_3D('',#5685,#4040,#4041);
#3464=AXIS2_PLACEMENT_3D('',#5689,#4044,#4045);
#3465=AXIS2_PLACEMENT_3D('',#5690,#4046,#4047);
#3466=AXIS2_PLACEMENT_3D('',#5691,#4048,#4049);
#3467=AXIS2_PLACEMENT_3D('',#5692,#4050,#4051);
#3468=AXIS2_PLACEMENT_3D('',#5693,#4052,#4053);
#3469=AXIS2_PLACEMENT_3D('',#5722,#4056,#4057);
#3470=AXIS2_PLACEMENT_3D('',#5723,#4058,#4059);
#3471=AXIS2_PLACEMENT_3D('',#5752,#4062,#4063);
#3472=AXIS2_PLACEMENT_3D('',#5753,#4064,#4065);
#3473=AXIS2_PLACEMENT_3D('',#5782,#4068,#4069);
#3474=AXIS2_PLACEMENT_3D('',#5783,#4070,#4071);
#3475=AXIS2_PLACEMENT_3D('',#5812,#4074,#4075);
#3476=AXIS2_PLACEMENT_3D('',#5813,#4076,#4077);
#3477=AXIS2_PLACEMENT_3D('',#5846,#4080,#4081);
#3478=AXIS2_PLACEMENT_3D('',#5847,#4082,#4083);
#3479=AXIS2_PLACEMENT_3D('',#5876,#4086,#4087);
#3480=AXIS2_PLACEMENT_3D('',#5877,#4088,#4089);
#3481=AXIS2_PLACEMENT_3D('',#5906,#4092,#4093);
#3482=AXIS2_PLACEMENT_3D('',#5907,#4094,#4095);
#3483=AXIS2_PLACEMENT_3D('',#5936,#4098,#4099);
#3484=AXIS2_PLACEMENT_3D('',#5937,#4100,#4101);
#3485=AXIS2_PLACEMENT_3D('',#5966,#4104,#4105);
#3486=AXIS2_PLACEMENT_3D('',#5967,#4106,#4107);
#3487=AXIS2_PLACEMENT_3D('',#5968,#4108,#4109);
#3488=AXIS2_PLACEMENT_3D('',#5969,#4110,#4111);
#3489=AXIS2_PLACEMENT_3D('',#5970,#4112,#4113);
#3490=AXIS2_PLACEMENT_3D('',#5971,#4114,#4115);
#3491=AXIS2_PLACEMENT_3D('',#5972,#4116,#4117);
#3492=AXIS2_PLACEMENT_3D('',#5973,#4118,#4119);
#3493=AXIS2_PLACEMENT_3D('',#5974,#4120,#4121);
#3494=AXIS2_PLACEMENT_3D('',#5975,#4122,#4123);
#3495=AXIS2_PLACEMENT_3D('',#5977,#4124,#4125);
#3496=AXIS2_PLACEMENT_3D('',#5979,#4126,#4127);
#3497=AXIS2_PLACEMENT_3D('',#5980,#4128,#4129);
#3498=AXIS2_PLACEMENT_3D('',#5982,#4130,#4131);
#3499=AXIS2_PLACEMENT_3D('',#5983,#4132,#4133);
#3500=AXIS2_PLACEMENT_3D('',#5985,#4134,#4135);
#3501=AXIS2_PLACEMENT_3D('',#5987,#4137,#4138);
#3502=AXIS2_PLACEMENT_3D('',#5988,#4139,#4140);
#3503=AXIS2_PLACEMENT_3D('',#5989,#4141,#4142);
#3504=AXIS2_PLACEMENT_3D('',#5990,#4143,#4144);
#3505=AXIS2_PLACEMENT_3D('',#5991,#4145,#4146);
#3506=AXIS2_PLACEMENT_3D('',#5992,#4147,#4148);
#3507=AXIS2_PLACEMENT_3D('',#5993,#4149,#4150);
#3508=AXIS2_PLACEMENT_3D('',#5994,#4151,#4152);
#3509=AXIS2_PLACEMENT_3D('',#5995,#4153,#4154);
#3510=AXIS2_PLACEMENT_3D('',#5996,#4155,#4156);
#3511=AXIS2_PLACEMENT_3D('',#5997,#4157,#4158);
#3512=AXIS2_PLACEMENT_3D('',#5998,#4159,#4160);
#3513=AXIS2_PLACEMENT_3D('',#5999,#4161,#4162);
#3514=AXIS2_PLACEMENT_3D('',#6000,#4163,#4164);
#3515=AXIS2_PLACEMENT_3D('',#6001,#4165,#4166);
#3516=AXIS2_PLACEMENT_3D('',#6002,#4167,#4168);
#3517=AXIS2_PLACEMENT_3D('',#6003,#4169,#4170);
#3518=AXIS2_PLACEMENT_3D('',#6005,#4171,#4172);
#3519=AXIS2_PLACEMENT_3D('',#6007,#4173,#4174);
#3520=AXIS2_PLACEMENT_3D('',#6021,#4175,#4176);
#3521=AXIS2_PLACEMENT_3D('',#6038,#4177,#4178);
#3522=AXIS2_PLACEMENT_3D('',#6040,#4180,#4181);
#3523=AXIS2_PLACEMENT_3D('',#6041,#4182,#4183);
#3524=AXIS2_PLACEMENT_3D('',#6042,#4184,#4185);
#3525=AXIS2_PLACEMENT_3D('',#6044,#4186,#4187);
#3526=AXIS2_PLACEMENT_3D('',#6046,#4189,#4190);
#3527=AXIS2_PLACEMENT_3D('',#6047,#4191,#4192);
#3528=AXIS2_PLACEMENT_3D('',#6048,#4193,#4194);
#3529=AXIS2_PLACEMENT_3D('',#6083,#4197,#4198);
#3530=AXIS2_PLACEMENT_3D('',#6118,#4201,#4202);
#3531=AXIS2_PLACEMENT_3D('',#6153,#4205,#4206);
#3532=AXIS2_PLACEMENT_3D('',#6188,#4209,#4210);
#3533=AXIS2_PLACEMENT_3D('',#6223,#4213,#4214);
#3534=AXIS2_PLACEMENT_3D('',#6258,#4217,#4218);
#3535=AXIS2_PLACEMENT_3D('',#6293,#4221,#4222);
#3536=AXIS2_PLACEMENT_3D('',#6328,#4225,#4226);
#3537=AXIS2_PLACEMENT_3D('',#6363,#4229,#4230);
#3538=AXIS2_PLACEMENT_3D('',#6398,#4233,#4234);
#3539=AXIS2_PLACEMENT_3D('',#6433,#4237,#4238);
#3540=AXIS2_PLACEMENT_3D('',#6468,#4241,#4242);
#3541=AXIS2_PLACEMENT_3D('',#6503,#4245,#4246);
#3542=AXIS2_PLACEMENT_3D('',#6538,#4249,#4250);
#3543=AXIS2_PLACEMENT_3D('',#6573,#4253,#4254);
#3544=AXIS2_PLACEMENT_3D('',#6608,#4257,#4258);
#3545=AXIS2_PLACEMENT_3D('',#6643,#4261,#4262);
#3546=AXIS2_PLACEMENT_3D('',#6678,#4265,#4266);
#3547=AXIS2_PLACEMENT_3D('',#6713,#4269,#4270);
#3548=AXIS2_PLACEMENT_3D('',#6748,#4273,#4274);
#3549=AXIS2_PLACEMENT_3D('',#6783,#4277,#4278);
#3550=AXIS2_PLACEMENT_3D('',#6818,#4281,#4282);
#3551=AXIS2_PLACEMENT_3D('',#6853,#4285,#4286);
#3552=AXIS2_PLACEMENT_3D('',#6888,#4289,#4290);
#3553=AXIS2_PLACEMENT_3D('',#6890,#4291,#4292);
#3554=AXIS2_PLACEMENT_3D('',#6902,#4294,#4295);
#3555=AXIS2_PLACEMENT_3D('',#6903,#4296,#4297);
#3556=AXIS2_PLACEMENT_3D('',#6904,#4298,#4299);
#3557=AXIS2_PLACEMENT_3D('',#6905,#4300,#4301);
#3558=AXIS2_PLACEMENT_3D('',#6906,#4302,#4303);
#3559=AXIS2_PLACEMENT_3D('',#6907,#4304,#4305);
#3560=AXIS2_PLACEMENT_3D('',#6908,#4306,#4307);
#3561=AXIS2_PLACEMENT_3D('',#6909,#4308,#4309);
#3562=AXIS2_PLACEMENT_3D('',#6910,#4310,#4311);
#3563=AXIS2_PLACEMENT_3D('',#6911,#4312,#4313);
#3564=AXIS2_PLACEMENT_3D('',#6912,#4314,#4315);
#3565=AXIS2_PLACEMENT_3D('',#6913,#4316,#4317);
#3566=AXIS2_PLACEMENT_3D('',#6914,#4318,#4319);
#3567=AXIS2_PLACEMENT_3D('',#6915,#4320,#4321);
#3568=AXIS2_PLACEMENT_3D('',#6916,#4322,#4323);
#3569=AXIS2_PLACEMENT_3D('',#6917,#4324,#4325);
#3570=AXIS2_PLACEMENT_3D('',#6918,#4326,#4327);
#3571=AXIS2_PLACEMENT_3D('',#6919,#4328,#4329);
#3572=AXIS2_PLACEMENT_3D('',#6920,#4330,#4331);
#3573=AXIS2_PLACEMENT_3D('',#6921,#4332,#4333);
#3574=AXIS2_PLACEMENT_3D('',#6922,#4334,#4335);
#3575=AXIS2_PLACEMENT_3D('',#6923,#4336,#4337);
#3576=AXIS2_PLACEMENT_3D('',#6924,#4338,#4339);
#3577=AXIS2_PLACEMENT_3D('',#6925,#4340,#4341);
#3578=AXIS2_PLACEMENT_3D('',#6927,#4342,#4343);
#3579=AXIS2_PLACEMENT_3D('',#6936,#4344,#4345);
#3580=AXIS2_PLACEMENT_3D('',#6938,#4346,#4347);
#3581=AXIS2_PLACEMENT_3D('',#6940,#4349,#4350);
#3582=AXIS2_PLACEMENT_3D('',#6943,#4352,#4353);
#3583=AXIS2_PLACEMENT_3D('',#6944,#4354,#4355);
#3584=AXIS2_PLACEMENT_3D('',#6945,#4356,#4357);
#3585=AXIS2_PLACEMENT_3D('',#6946,#4358,#4359);
#3586=AXIS2_PLACEMENT_3D('',#6947,#4360,#4361);
#3587=AXIS2_PLACEMENT_3D('',#6948,#4362,#4363);
#3588=AXIS2_PLACEMENT_3D('',#6949,#4364,#4365);
#3589=AXIS2_PLACEMENT_3D('',#6950,#4366,#4367);
#3590=AXIS2_PLACEMENT_3D('',#6951,#4368,#4369);
#3591=AXIS2_PLACEMENT_3D('',#6952,#4370,#4371);
#3592=AXIS2_PLACEMENT_3D('',#6953,#4372,#4373);
#3593=AXIS2_PLACEMENT_3D('',#6954,#4374,#4375);
#3594=AXIS2_PLACEMENT_3D('',#6955,#4376,#4377);
#3595=AXIS2_PLACEMENT_3D('',#6956,#4378,#4379);
#3596=AXIS2_PLACEMENT_3D('',#6957,#4380,#4381);
#3597=AXIS2_PLACEMENT_3D('',#6958,#4382,#4383);
#3598=AXIS2_PLACEMENT_3D('',#6959,#4384,#4385);
#3599=AXIS2_PLACEMENT_3D('',#6960,#4386,#4387);
#3600=AXIS2_PLACEMENT_3D('',#6961,#4388,#4389);
#3601=AXIS2_PLACEMENT_3D('',#6962,#4390,#4391);
#3602=AXIS2_PLACEMENT_3D('',#6963,#4392,#4393);
#3603=AXIS2_PLACEMENT_3D('',#6964,#4394,#4395);
#3604=AXIS2_PLACEMENT_3D('',#6965,#4396,#4397);
#3605=AXIS2_PLACEMENT_3D('',#6966,#4398,#4399);
#3606=AXIS2_PLACEMENT_3D('',#6967,#4400,#4401);
#3607=AXIS2_PLACEMENT_3D('',#6968,#4402,#4403);
#3608=AXIS2_PLACEMENT_3D('',#6969,#4404,#4405);
#3609=AXIS2_PLACEMENT_3D('',#6970,#4406,#4407);
#3610=AXIS2_PLACEMENT_3D('',#6971,#4408,#4409);
#3611=AXIS2_PLACEMENT_3D('',#6972,#4410,#4411);
#3612=AXIS2_PLACEMENT_3D('',#6973,#4412,#4413);
#3613=AXIS2_PLACEMENT_3D('',#6974,#4414,#4415);
#3614=AXIS2_PLACEMENT_3D('',#6975,#4416,#4417);
#3615=AXIS2_PLACEMENT_3D('',#6976,#4418,#4419);
#3616=AXIS2_PLACEMENT_3D('',#6977,#4420,#4421);
#3617=AXIS2_PLACEMENT_3D('',#6978,#4422,#4423);
#3618=AXIS2_PLACEMENT_3D('',#6979,#4424,#4425);
#3619=AXIS2_PLACEMENT_3D('',#6980,#4426,#4427);
#3620=AXIS2_PLACEMENT_3D('',#6981,#4428,#4429);
#3621=AXIS2_PLACEMENT_3D('',#6982,#4430,#4431);
#3622=AXIS2_PLACEMENT_3D('',#6983,#4432,#4433);
#3623=AXIS2_PLACEMENT_3D('',#6984,#4434,#4435);
#3624=AXIS2_PLACEMENT_3D('',#6985,#4436,#4437);
#3625=AXIS2_PLACEMENT_3D('',#6986,#4438,#4439);
#3626=AXIS2_PLACEMENT_3D('',#6987,#4440,#4441);
#3627=AXIS2_PLACEMENT_3D('',#6988,#4442,#4443);
#3628=AXIS2_PLACEMENT_3D('',#7006,#4444,#4445);
#3629=AXIS2_PLACEMENT_3D('',#7008,#4446,#4447);
#3630=AXIS2_PLACEMENT_3D('',#7010,#4449,#4450);
#3631=AXIS2_PLACEMENT_3D('',#7011,#4451,#4452);
#3632=AXIS2_PLACEMENT_3D('',#7013,#4453,#4454);
#3633=AXIS2_PLACEMENT_3D('',#7014,#4455,#4456);
#3634=AXIS2_PLACEMENT_3D('',#7016,#4457,#4458);
#3635=AXIS2_PLACEMENT_3D('',#7018,#4460,#4461);
#3636=AXIS2_PLACEMENT_3D('',#7019,#4462,#4463);
#3637=AXIS2_PLACEMENT_3D('',#7021,#4465,#4466);
#3638=AXIS2_PLACEMENT_3D('',#7022,#4467,#4468);
#3639=AXIS2_PLACEMENT_3D('',#7023,#4469,#4470);
#3640=AXIS2_PLACEMENT_3D('',#7026,#4471,#4472);
#3641=AXIS2_PLACEMENT_3D('',#7027,#4473,#4474);
#3642=AXIS2_PLACEMENT_3D('',#7031,#4476,#4477);
#3643=AXIS2_PLACEMENT_3D('',#7032,#4478,#4479);
#3644=AXIS2_PLACEMENT_3D('',#7075,#4482,#4483);
#3645=AXIS2_PLACEMENT_3D('',#7081,#4487,#4488);
#3646=AXIS2_PLACEMENT_3D('',#7105,#4490,#4491);
#3647=AXIS2_PLACEMENT_3D('',#7131,#4493,#4494);
#3648=AXIS2_PLACEMENT_3D('',#7150,#4495,#4496);
#3649=AXIS2_PLACEMENT_3D('',#7151,#4497,#4498);
#3650=AXIS2_PLACEMENT_3D('',#7155,#4501,#4502);
#3651=AXIS2_PLACEMENT_3D('',#7177,#4503,#4504);
#3652=AXIS2_PLACEMENT_3D('',#7180,#4505,#4506);
#3653=AXIS2_PLACEMENT_3D('',#7181,#4507,#4508);
#3654=AXIS2_PLACEMENT_3D('',#7184,#4510,#4511);
#3655=AXIS2_PLACEMENT_3D('',#7185,#4512,#4513);
#3656=AXIS2_PLACEMENT_3D('',#7187,#4514,#4515);
#3657=AXIS2_PLACEMENT_3D('',#7188,#4516,#4517);
#3658=AXIS2_PLACEMENT_3D('',#7190,#4518,#4519);
#3659=AXIS2_PLACEMENT_3D('',#7192,#4521,#4522);
#3660=AXIS2_PLACEMENT_3D('',#7194,#4523,#4524);
#3661=AXIS2_PLACEMENT_3D('',#7196,#4525,#4526);
#3662=AXIS2_PLACEMENT_3D('',#7197,#4527,#4528);
#3663=AXIS2_PLACEMENT_3D('',#7198,#4529,#4530);
#3664=AXIS2_PLACEMENT_3D('',#7203,#4534,#4535);
#3665=AXIS2_PLACEMENT_3D('',#7204,#4536,#4537);
#3666=AXIS2_PLACEMENT_3D('',#7205,#4538,#4539);
#3667=AXIS2_PLACEMENT_3D('',#7207,#4540,#4541);
#3668=AXIS2_PLACEMENT_3D('',#7208,#4542,#4543);
#3669=AXIS2_PLACEMENT_3D('',#7209,#4544,#4545);
#3670=AXIS2_PLACEMENT_3D('',#7210,#4546,#4547);
#3671=AXIS2_PLACEMENT_3D('',#7212,#4548,#4549);
#3672=AXIS2_PLACEMENT_3D('',#7213,#4550,#4551);
#3673=AXIS2_PLACEMENT_3D('',#7215,#4553,#4554);
#3674=AXIS2_PLACEMENT_3D('',#7216,#4555,#4556);
#3675=AXIS2_PLACEMENT_3D('',#7219,#4557,#4558);
#3676=AXIS2_PLACEMENT_3D('',#7221,#4559,#4560);
#3677=AXIS2_PLACEMENT_3D('',#7222,#4561,#4562);
#3678=AXIS2_PLACEMENT_3D('',#7224,#4563,#4564);
#3679=AXIS2_PLACEMENT_3D('',#7225,#4565,#4566);
#3680=AXIS2_PLACEMENT_3D('',#7227,#4567,#4568);
#3681=AXIS2_PLACEMENT_3D('',#7228,#4569,#4570);
#3682=AXIS2_PLACEMENT_3D('',#7230,#4571,#4572);
#3683=AXIS2_PLACEMENT_3D('',#7231,#4573,#4574);
#3684=AXIS2_PLACEMENT_3D('',#7233,#4576,#4577);
#3685=AXIS2_PLACEMENT_3D('',#7234,#4578,#4579);
#3686=AXIS2_PLACEMENT_3D('',#7236,#4580,#4581);
#3687=AXIS2_PLACEMENT_3D('',#7239,#4583,#4584);
#3688=AXIS2_PLACEMENT_3D('',#7240,#4585,#4586);
#3689=AXIS2_PLACEMENT_3D('',#7242,#4587,#4588);
#3690=AXIS2_PLACEMENT_3D('',#7243,#4589,#4590);
#3691=AXIS2_PLACEMENT_3D('',#7245,#4591,#4592);
#3692=AXIS2_PLACEMENT_3D('',#7247,#4594,#4595);
#3693=AXIS2_PLACEMENT_3D('',#7249,#4596,#4597);
#3694=AXIS2_PLACEMENT_3D('',#7250,#4598,#4599);
#3695=AXIS2_PLACEMENT_3D('',#7252,#4601,#4602);
#3696=AXIS2_PLACEMENT_3D('',#7253,#4603,#4604);
#3697=AXIS2_PLACEMENT_3D('',#7254,#4605,#4606);
#3698=AXIS2_PLACEMENT_3D('',#7257,#4607,#4608);
#3699=AXIS2_PLACEMENT_3D('',#7258,#4609,#4610);
#3700=AXIS2_PLACEMENT_3D('',#7259,#4611,#4612);
#3701=AXIS2_PLACEMENT_3D('',#7261,#4613,#4614);
#3702=AXIS2_PLACEMENT_3D('',#7264,#4616,#4617);
#3703=AXIS2_PLACEMENT_3D('',#7265,#4618,#4619);
#3704=AXIS2_PLACEMENT_3D('',#7266,#4620,#4621);
#3705=AXIS2_PLACEMENT_3D('',#7267,#4622,#4623);
#3706=AXIS2_PLACEMENT_3D('',#7268,#4624,#4625);
#3707=AXIS2_PLACEMENT_3D('',#7270,#4626,#4627);
#3708=AXIS2_PLACEMENT_3D('',#7273,#4629,#4630);
#3709=AXIS2_PLACEMENT_3D('',#7274,#4631,#4632);
#3710=AXIS2_PLACEMENT_3D('',#7276,#4633,#4634);
#3711=AXIS2_PLACEMENT_3D('',#7279,#4636,#4637);
#3712=AXIS2_PLACEMENT_3D('',#7280,#4638,#4639);
#3713=AXIS2_PLACEMENT_3D('',#7281,#4640,#4641);
#3714=AXIS2_PLACEMENT_3D('',#7282,#4642,#4643);
#3715=AXIS2_PLACEMENT_3D('',#7283,#4644,#4645);
#3716=AXIS2_PLACEMENT_3D('',#7284,#4646,#4647);
#3717=AXIS2_PLACEMENT_3D('',#7285,#4648,#4649);
#3718=AXIS2_PLACEMENT_3D('',#7286,#4650,#4651);
#3719=AXIS2_PLACEMENT_3D('',#7287,#4652,#4653);
#3720=AXIS2_PLACEMENT_3D('',#7288,#4654,#4655);
#3721=AXIS2_PLACEMENT_3D('',#7289,#4656,#4657);
#3722=AXIS2_PLACEMENT_3D('',#7290,#4658,#4659);
#3723=AXIS2_PLACEMENT_3D('',#7291,#4660,#4661);
#3724=DIRECTION('axis',(0.,0.,1.));
#3725=DIRECTION('refdir',(1.,0.,0.));
#3726=DIRECTION('axis',(0.,0.,1.));
#3727=DIRECTION('refdir',(1.,0.,0.));
#3728=DIRECTION('center_axis',(1.,0.,0.));
#3729=DIRECTION('ref_axis',(0.,0.,-1.));
#3730=DIRECTION('center_axis',(-1.,0.,0.));
#3731=DIRECTION('ref_axis',(0.,1.22464679914735E-16,1.));
#3732=DIRECTION('center_axis',(0.,-1.,-1.22464679914735E-16));
#3733=DIRECTION('ref_axis',(0.,-1.22464679914735E-16,1.));
#3734=DIRECTION('center_axis',(1.,0.,0.));
#3735=DIRECTION('ref_axis',(0.,1.22464679914735E-16,1.));
#3736=DIRECTION('center_axis',(-1.,0.,0.));
#3737=DIRECTION('ref_axis',(0.,0.,1.));
#3738=DIRECTION('center_axis',(1.,0.,0.));
#3739=DIRECTION('ref_axis',(0.,0.,-1.));
#3740=DIRECTION('center_axis',(1.,0.,0.));
#3741=DIRECTION('ref_axis',(0.,0.,-1.));
#3742=DIRECTION('center_axis',(1.,0.,0.));
#3743=DIRECTION('ref_axis',(0.,0.,-1.));
#3744=DIRECTION('',(-1.,0.,0.));
#3745=DIRECTION('center_axis',(-1.,0.,0.));
#3746=DIRECTION('ref_axis',(0.,0.968583161128631,-0.248689887164855));
#3747=DIRECTION('',(-1.,0.,0.));
#3748=DIRECTION('',(1.,0.,0.));
#3749=DIRECTION('center_axis',(-1.,0.,0.));
#3750=DIRECTION('ref_axis',(0.,0.876306680043864,-0.481753674101715));
#3751=DIRECTION('',(-1.,0.,0.));
#3752=DIRECTION('',(1.,0.,0.));
#3753=DIRECTION('center_axis',(-1.,0.,0.));
#3754=DIRECTION('ref_axis',(0.,0.728968627421412,-0.684547105928688));
#3755=DIRECTION('',(-1.,0.,0.));
#3756=DIRECTION('',(1.,0.,0.));
#3757=DIRECTION('center_axis',(-1.,0.,0.));
#3758=DIRECTION('ref_axis',(0.,0.535826794978997,-0.844327925502015));
#3759=DIRECTION('',(-1.,0.,0.));
#3760=DIRECTION('',(1.,0.,0.));
#3761=DIRECTION('center_axis',(-1.,0.,0.));
#3762=DIRECTION('ref_axis',(0.,0.309016994374947,-0.951056516295154));
#3763=DIRECTION('',(-1.,0.,0.));
#3764=DIRECTION('',(1.,0.,0.));
#3765=DIRECTION('center_axis',(-1.,0.,0.));
#3766=DIRECTION('ref_axis',(0.,0.0627905195293137,-0.998026728428272));
#3767=DIRECTION('',(-1.,0.,0.));
#3768=DIRECTION('',(1.,0.,0.));
#3769=DIRECTION('center_axis',(-1.,0.,0.));
#3770=DIRECTION('ref_axis',(0.,-0.187381314585725,-0.982287250728689));
#3771=DIRECTION('',(-1.,0.,0.));
#3772=DIRECTION('',(1.,0.,0.));
#3773=DIRECTION('center_axis',(-1.,0.,0.));
#3774=DIRECTION('ref_axis',(0.,-0.425779291565072,-0.90482705246602));
#3775=DIRECTION('',(-1.,0.,0.));
#3776=DIRECTION('',(1.,0.,0.));
#3777=DIRECTION('center_axis',(-1.,0.,0.));
#3778=DIRECTION('ref_axis',(0.,-0.637423989748689,-0.770513242775789));
#3779=DIRECTION('',(-1.,0.,0.));
#3780=DIRECTION('',(1.,0.,0.));
#3781=DIRECTION('center_axis',(-1.,0.,0.));
#3782=DIRECTION('ref_axis',(0.,-0.809016994374947,-0.587785252292473));
#3783=DIRECTION('',(-1.,0.,0.));
#3784=DIRECTION('',(1.,0.,0.));
#3785=DIRECTION('center_axis',(-1.,0.,0.));
#3786=DIRECTION('ref_axis',(0.,-0.929776485888251,-0.368124552684678));
#3787=DIRECTION('',(-1.,0.,0.));
#3788=DIRECTION('',(1.,0.,0.));
#3789=DIRECTION('center_axis',(-1.,0.,0.));
#3790=DIRECTION('ref_axis',(0.,-0.992114701314478,-0.125333233564304));
#3791=DIRECTION('',(-1.,0.,0.));
#3792=DIRECTION('',(1.,0.,0.));
#3793=DIRECTION('center_axis',(-1.,0.,0.));
#3794=DIRECTION('ref_axis',(0.,-0.992114701314478,0.125333233564304));
#3795=DIRECTION('',(-1.,0.,0.));
#3796=DIRECTION('',(1.,0.,0.));
#3797=DIRECTION('center_axis',(-1.,0.,0.));
#3798=DIRECTION('ref_axis',(0.,-0.929776485888251,0.368124552684678));
#3799=DIRECTION('',(-1.,0.,0.));
#3800=DIRECTION('',(1.,0.,0.));
#3801=DIRECTION('center_axis',(-1.,0.,0.));
#3802=DIRECTION('ref_axis',(0.,-0.809016994374947,0.587785252292473));
#3803=DIRECTION('',(-1.,0.,0.));
#3804=DIRECTION('',(1.,0.,0.));
#3805=DIRECTION('center_axis',(-1.,0.,0.));
#3806=DIRECTION('ref_axis',(0.,-0.63742398974869,0.770513242775789));
#3807=DIRECTION('',(-1.,0.,0.));
#3808=DIRECTION('',(1.,0.,0.));
#3809=DIRECTION('center_axis',(-1.,0.,0.));
#3810=DIRECTION('ref_axis',(0.,-0.425779291565073,0.904827052466019));
#3811=DIRECTION('',(-1.,0.,0.));
#3812=DIRECTION('',(1.,0.,0.));
#3813=DIRECTION('center_axis',(-1.,0.,0.));
#3814=DIRECTION('ref_axis',(0.,-0.187381314585725,0.982287250728689));
#3815=DIRECTION('',(-1.,0.,0.));
#3816=DIRECTION('',(1.,0.,0.));
#3817=DIRECTION('center_axis',(-1.,0.,0.));
#3818=DIRECTION('ref_axis',(0.,0.0627905195293132,0.998026728428272));
#3819=DIRECTION('',(-1.,0.,0.));
#3820=DIRECTION('',(1.,0.,0.));
#3821=DIRECTION('center_axis',(-1.,0.,0.));
#3822=DIRECTION('ref_axis',(0.,0.309016994374947,0.951056516295154));
#3823=DIRECTION('',(-1.,0.,0.));
#3824=DIRECTION('',(1.,0.,0.));
#3825=DIRECTION('center_axis',(-1.,0.,0.));
#3826=DIRECTION('ref_axis',(0.,0.535826794978997,0.844327925502015));
#3827=DIRECTION('',(-1.,0.,0.));
#3828=DIRECTION('',(1.,0.,0.));
#3829=DIRECTION('center_axis',(-1.,0.,0.));
#3830=DIRECTION('ref_axis',(0.,0.728968627421412,0.684547105928689));
#3831=DIRECTION('',(-1.,0.,0.));
#3832=DIRECTION('',(1.,0.,0.));
#3833=DIRECTION('center_axis',(-1.,0.,0.));
#3834=DIRECTION('ref_axis',(0.,0.876306680043864,0.481753674101715));
#3835=DIRECTION('',(-1.,0.,0.));
#3836=DIRECTION('',(1.,0.,0.));
#3837=DIRECTION('center_axis',(-1.,0.,0.));
#3838=DIRECTION('ref_axis',(0.,0.968583161128631,0.248689887164855));
#3839=DIRECTION('',(-1.,0.,0.));
#3840=DIRECTION('',(1.,0.,0.));
#3841=DIRECTION('center_axis',(-1.,0.,0.));
#3842=DIRECTION('ref_axis',(0.,0.,-1.));
#3843=DIRECTION('center_axis',(1.,0.,0.));
#3844=DIRECTION('ref_axis',(0.,0.,-1.));
#3845=DIRECTION('',(-0.707106781186546,-8.65956056235495E-17,0.707106781186549));
#3846=DIRECTION('center_axis',(1.,0.,0.));
#3847=DIRECTION('ref_axis',(0.,0.,-1.));
#3848=DIRECTION('center_axis',(1.,0.,0.));
#3849=DIRECTION('ref_axis',(0.,0.,-1.));
#3850=DIRECTION('center_axis',(1.,0.,0.));
#3851=DIRECTION('ref_axis',(0.,0.,-1.));
#3852=DIRECTION('center_axis',(1.,0.,0.));
#3853=DIRECTION('ref_axis',(0.,0.,-1.));
#3854=DIRECTION('center_axis',(1.,0.,0.));
#3855=DIRECTION('ref_axis',(0.,0.,-1.));
#3856=DIRECTION('center_axis',(1.,0.,0.));
#3857=DIRECTION('ref_axis',(0.,0.,-1.));
#3858=DIRECTION('center_axis',(1.,0.,0.));
#3859=DIRECTION('ref_axis',(0.,0.,-1.));
#3860=DIRECTION('center_axis',(1.,0.,0.));
#3861=DIRECTION('ref_axis',(0.,0.,-1.));
#3862=DIRECTION('center_axis',(1.,0.,0.));
#3863=DIRECTION('ref_axis',(0.,0.,-1.));
#3864=DIRECTION('center_axis',(1.,0.,0.));
#3865=DIRECTION('ref_axis',(0.,0.,-1.));
#3866=DIRECTION('center_axis',(1.,0.,0.));
#3867=DIRECTION('ref_axis',(0.,0.,-1.));
#3868=DIRECTION('center_axis',(1.,0.,0.));
#3869=DIRECTION('ref_axis',(0.,0.,-1.));
#3870=DIRECTION('center_axis',(1.,0.,0.));
#3871=DIRECTION('ref_axis',(0.,0.,-1.));
#3872=DIRECTION('center_axis',(1.,0.,0.));
#3873=DIRECTION('ref_axis',(0.,0.,-1.));
#3874=DIRECTION('center_axis',(1.,0.,0.));
#3875=DIRECTION('ref_axis',(0.,0.,-1.));
#3876=DIRECTION('center_axis',(1.,0.,0.));
#3877=DIRECTION('ref_axis',(0.,0.,-1.));
#3878=DIRECTION('center_axis',(1.,0.,0.));
#3879=DIRECTION('ref_axis',(0.,0.,-1.));
#3880=DIRECTION('center_axis',(1.,0.,0.));
#3881=DIRECTION('ref_axis',(0.,0.,-1.));
#3882=DIRECTION('center_axis',(1.,0.,0.));
#3883=DIRECTION('ref_axis',(0.,0.,-1.));
#3884=DIRECTION('center_axis',(1.,0.,0.));
#3885=DIRECTION('ref_axis',(0.,0.,-1.));
#3886=DIRECTION('center_axis',(1.,0.,0.));
#3887=DIRECTION('ref_axis',(0.,0.,-1.));
#3888=DIRECTION('center_axis',(1.,0.,0.));
#3889=DIRECTION('ref_axis',(0.,0.,-1.));
#3890=DIRECTION('center_axis',(1.,0.,0.));
#3891=DIRECTION('ref_axis',(0.,0.,-1.));
#3892=DIRECTION('center_axis',(1.,0.,0.));
#3893=DIRECTION('ref_axis',(0.,0.,-1.));
#3894=DIRECTION('center_axis',(1.,0.,0.));
#3895=DIRECTION('ref_axis',(0.,0.,-1.));
#3896=DIRECTION('center_axis',(1.,0.,0.));
#3897=DIRECTION('ref_axis',(0.,0.,-1.));
#3898=DIRECTION('center_axis',(1.,0.,0.));
#3899=DIRECTION('ref_axis',(0.,0.,-1.));
#3900=DIRECTION('',(1.,0.,0.));
#3901=DIRECTION('center_axis',(1.,0.,0.));
#3902=DIRECTION('ref_axis',(0.,0.,-1.));
#3903=DIRECTION('',(-1.,0.,0.));
#3904=DIRECTION('center_axis',(1.,0.,0.));
#3905=DIRECTION('ref_axis',(0.,0.,-1.));
#3906=DIRECTION('center_axis',(1.,0.,0.));
#3907=DIRECTION('ref_axis',(0.,0.,-1.));
#3908=DIRECTION('center_axis',(1.,0.,0.));
#3909=DIRECTION('ref_axis',(0.,0.,-1.));
#3910=DIRECTION('center_axis',(1.,0.,0.));
#3911=DIRECTION('ref_axis',(0.,0.,-1.));
#3912=DIRECTION('center_axis',(1.,0.,0.));
#3913=DIRECTION('ref_axis',(0.,0.,-1.));
#3914=DIRECTION('center_axis',(1.,0.,0.));
#3915=DIRECTION('ref_axis',(0.,0.,-1.));
#3916=DIRECTION('center_axis',(1.,0.,0.));
#3917=DIRECTION('ref_axis',(0.,0.,-1.));
#3918=DIRECTION('center_axis',(1.,0.,0.));
#3919=DIRECTION('ref_axis',(0.,0.,-1.));
#3920=DIRECTION('center_axis',(1.,0.,0.));
#3921=DIRECTION('ref_axis',(0.,0.,-1.));
#3922=DIRECTION('center_axis',(1.,0.,0.));
#3923=DIRECTION('ref_axis',(0.,0.,-1.));
#3924=DIRECTION('center_axis',(1.,0.,0.));
#3925=DIRECTION('ref_axis',(0.,0.,-1.));
#3926=DIRECTION('center_axis',(1.,0.,0.));
#3927=DIRECTION('ref_axis',(0.,0.,-1.));
#3928=DIRECTION('center_axis',(1.,0.,0.));
#3929=DIRECTION('ref_axis',(0.,0.,-1.));
#3930=DIRECTION('center_axis',(1.,0.,0.));
#3931=DIRECTION('ref_axis',(0.,0.,-1.));
#3932=DIRECTION('center_axis',(1.,0.,0.));
#3933=DIRECTION('ref_axis',(0.,0.,-1.));
#3934=DIRECTION('center_axis',(1.,0.,0.));
#3935=DIRECTION('ref_axis',(0.,0.,-1.));
#3936=DIRECTION('center_axis',(1.,0.,0.));
#3937=DIRECTION('ref_axis',(0.,0.,-1.));
#3938=DIRECTION('center_axis',(1.,0.,0.));
#3939=DIRECTION('ref_axis',(0.,0.,-1.));
#3940=DIRECTION('center_axis',(1.,0.,0.));
#3941=DIRECTION('ref_axis',(0.,0.,-1.));
#3942=DIRECTION('center_axis',(1.,0.,0.));
#3943=DIRECTION('ref_axis',(0.,0.,-1.));
#3944=DIRECTION('center_axis',(1.,0.,0.));
#3945=DIRECTION('ref_axis',(0.,0.,-1.));
#3946=DIRECTION('center_axis',(1.,0.,0.));
#3947=DIRECTION('ref_axis',(0.,0.,-1.));
#3948=DIRECTION('center_axis',(1.,0.,0.));
#3949=DIRECTION('ref_axis',(0.,0.,-1.));
#3950=DIRECTION('center_axis',(1.,0.,0.));
#3951=DIRECTION('ref_axis',(0.,0.,-1.));
#3952=DIRECTION('center_axis',(1.,0.,0.));
#3953=DIRECTION('ref_axis',(0.,0.,-1.));
#3954=DIRECTION('center_axis',(1.,0.,0.));
#3955=DIRECTION('ref_axis',(0.,0.,-1.));
#3956=DIRECTION('center_axis',(1.,0.,0.));
#3957=DIRECTION('ref_axis',(0.,0.,-1.));
#3958=DIRECTION('center_axis',(1.,0.,0.));
#3959=DIRECTION('ref_axis',(0.,0.,-1.));
#3960=DIRECTION('center_axis',(1.,0.,0.));
#3961=DIRECTION('ref_axis',(0.,0.,-1.));
#3962=DIRECTION('center_axis',(1.,0.,0.));
#3963=DIRECTION('ref_axis',(0.,0.,-1.));
#3964=DIRECTION('center_axis',(1.,0.,0.));
#3965=DIRECTION('ref_axis',(0.,0.,-1.));
#3966=DIRECTION('center_axis',(1.,0.,0.));
#3967=DIRECTION('ref_axis',(0.,0.,-1.));
#3968=DIRECTION('center_axis',(1.,0.,0.));
#3969=DIRECTION('ref_axis',(0.,0.,-1.));
#3970=DIRECTION('center_axis',(1.,0.,0.));
#3971=DIRECTION('ref_axis',(0.,0.,-1.));
#3972=DIRECTION('center_axis',(1.,0.,0.));
#3973=DIRECTION('ref_axis',(0.,0.,-1.));
#3974=DIRECTION('center_axis',(1.,0.,0.));
#3975=DIRECTION('ref_axis',(0.,0.,-1.));
#3976=DIRECTION('center_axis',(1.,0.,0.));
#3977=DIRECTION('ref_axis',(0.,0.,-1.));
#3978=DIRECTION('center_axis',(1.,0.,0.));
#3979=DIRECTION('ref_axis',(0.,0.,-1.));
#3980=DIRECTION('center_axis',(1.,0.,0.));
#3981=DIRECTION('ref_axis',(0.,0.,-1.));
#3982=DIRECTION('center_axis',(1.,0.,0.));
#3983=DIRECTION('ref_axis',(0.,0.,-1.));
#3984=DIRECTION('center_axis',(1.,0.,0.));
#3985=DIRECTION('ref_axis',(0.,0.,-1.));
#3986=DIRECTION('center_axis',(1.,0.,0.));
#3987=DIRECTION('ref_axis',(0.,0.,-1.));
#3988=DIRECTION('center_axis',(1.,0.,0.));
#3989=DIRECTION('ref_axis',(0.,0.,-1.));
#3990=DIRECTION('center_axis',(1.,0.,0.));
#3991=DIRECTION('ref_axis',(0.,0.,-1.));
#3992=DIRECTION('center_axis',(1.,0.,0.));
#3993=DIRECTION('ref_axis',(0.,0.,-1.));
#3994=DIRECTION('center_axis',(-1.,0.,0.));
#3995=DIRECTION('ref_axis',(0.,1.,0.));
#3996=DIRECTION('center_axis',(1.,0.,0.));
#3997=DIRECTION('ref_axis',(0.,0.,-1.));
#3998=DIRECTION('center_axis',(1.,0.,0.));
#3999=DIRECTION('ref_axis',(0.,0.,-1.));
#4000=DIRECTION('',(-0.702378778976759,8.71707730133816E-17,-0.7118033793423));
#4001=DIRECTION('center_axis',(1.,0.,0.));
#4002=DIRECTION('ref_axis',(0.,0.,-1.));
#4003=DIRECTION('center_axis',(1.,0.,0.));
#4004=DIRECTION('ref_axis',(0.,0.,-1.));
#4005=DIRECTION('center_axis',(-1.,0.,0.));
#4006=DIRECTION('ref_axis',(0.,0.,1.));
#4007=DIRECTION('center_axis',(1.,0.,0.));
#4008=DIRECTION('ref_axis',(0.,0.,-1.));
#4009=DIRECTION('center_axis',(1.,0.,0.));
#4010=DIRECTION('ref_axis',(0.,0.,-1.));
#4011=DIRECTION('',(-1.,0.,0.));
#4012=DIRECTION('axis',(0.,0.,1.));
#4013=DIRECTION('refdir',(1.,0.,0.));
#4014=DIRECTION('center_axis',(-1.,0.,0.));
#4015=DIRECTION('ref_axis',(0.,1.83697019872103E-16,-1.));
#4016=DIRECTION('center_axis',(-1.,0.,0.));
#4017=DIRECTION('ref_axis',(0.,-1.,0.));
#4018=DIRECTION('center_axis',(1.,0.,0.));
#4019=DIRECTION('ref_axis',(0.,-1.,0.));
#4020=DIRECTION('center_axis',(-1.,0.,0.));
#4021=DIRECTION('ref_axis',(0.,-1.,0.));
#4022=DIRECTION('',(0.,0.,-1.));
#4023=DIRECTION('center_axis',(-1.,0.,0.));
#4024=DIRECTION('ref_axis',(0.,-1.,0.));
#4025=DIRECTION('',(0.,0.,1.));
#4026=DIRECTION('center_axis',(0.,-1.,0.));
#4027=DIRECTION('ref_axis',(0.,0.,-1.));
#4028=DIRECTION('',(1.,0.,0.));
#4029=DIRECTION('',(0.,0.,-1.));
#4030=DIRECTION('',(1.,0.,0.));
#4031=DIRECTION('center_axis',(1.,0.,0.));
#4032=DIRECTION('ref_axis',(0.,-6.12323399573677E-17,-1.));
#4033=DIRECTION('center_axis',(1.,0.,0.));
#4034=DIRECTION('ref_axis',(0.,-1.,0.));
#4035=DIRECTION('center_axis',(-1.,0.,0.));
#4036=DIRECTION('ref_axis',(0.,-1.,0.));
#4037=DIRECTION('center_axis',(1.,0.,0.));
#4038=DIRECTION('ref_axis',(0.,-2.83276944882399E-16,-1.));
#4039=DIRECTION('',(-1.,0.,0.));
#4040=DIRECTION('center_axis',(0.,1.,0.));
#4041=DIRECTION('ref_axis',(0.,0.,1.));
#4042=DIRECTION('',(1.,0.,0.));
#4043=DIRECTION('',(0.,0.,1.));
#4044=DIRECTION('center_axis',(1.,0.,0.));
#4045=DIRECTION('ref_axis',(0.,-6.12323399573677E-17,-1.));
#4046=DIRECTION('center_axis',(-1.,0.,0.));
#4047=DIRECTION('ref_axis',(0.,-1.,0.));
#4048=DIRECTION('center_axis',(-1.,0.,0.));
#4049=DIRECTION('ref_axis',(0.,-1.,0.));
#4050=DIRECTION('axis',(0.,0.,1.));
#4051=DIRECTION('refdir',(1.,0.,0.));
#4052=DIRECTION('center_axis',(0.,0.,-1.));
#4053=DIRECTION('ref_axis',(0.809016994374947,-0.587785252292473,0.));
#4054=DIRECTION('',(0.,0.,-1.));
#4055=DIRECTION('',(0.,0.,1.));
#4056=DIRECTION('center_axis',(0.,0.,1.));
#4057=DIRECTION('ref_axis',(-0.809016994374947,0.587785252292473,0.));
#4058=DIRECTION('center_axis',(0.,0.,-1.));
#4059=DIRECTION('ref_axis',(0.309016994374946,-0.951056516295154,0.));
#4060=DIRECTION('',(0.,0.,-1.));
#4061=DIRECTION('',(0.,0.,1.));
#4062=DIRECTION('center_axis',(0.,0.,1.));
#4063=DIRECTION('ref_axis',(-0.309016994374947,0.951056516295154,0.));
#4064=DIRECTION('center_axis',(0.,0.,-1.));
#4065=DIRECTION('ref_axis',(-0.309016994374949,-0.951056516295153,0.));
#4066=DIRECTION('',(0.,0.,-1.));
#4067=DIRECTION('',(0.,0.,1.));
#4068=DIRECTION('center_axis',(0.,0.,1.));
#4069=DIRECTION('ref_axis',(0.309016994374948,0.951056516295154,0.));
#4070=DIRECTION('center_axis',(0.,0.,-1.));
#4071=DIRECTION('ref_axis',(-0.809016994374947,-0.587785252292474,0.));
#4072=DIRECTION('',(0.,0.,-1.));
#4073=DIRECTION('',(0.,0.,1.));
#4074=DIRECTION('center_axis',(0.,0.,1.));
#4075=DIRECTION('ref_axis',(0.809016994374947,0.587785252292473,0.));
#4076=DIRECTION('center_axis',(0.,0.,-1.));
#4077=DIRECTION('ref_axis',(-1.,2.6124255799288E-16,0.));
#4078=DIRECTION('',(0.,0.,-1.));
#4079=DIRECTION('',(0.,0.,1.));
#4080=DIRECTION('center_axis',(0.,0.,1.));
#4081=DIRECTION('ref_axis',(1.,-1.38777878078144E-16,0.));
#4082=DIRECTION('center_axis',(0.,0.,-1.));
#4083=DIRECTION('ref_axis',(-0.809016994374947,0.587785252292473,0.));
#4084=DIRECTION('',(0.,0.,-1.));
#4085=DIRECTION('',(0.,0.,1.));
#4086=DIRECTION('center_axis',(0.,0.,1.));
#4087=DIRECTION('ref_axis',(0.809016994374947,-0.587785252292473,0.));
#4088=DIRECTION('center_axis',(0.,0.,-1.));
#4089=DIRECTION('ref_axis',(-0.309016994374946,0.951056516295154,0.));
#4090=DIRECTION('',(0.,0.,-1.));
#4091=DIRECTION('',(0.,0.,1.));
#4092=DIRECTION('center_axis',(0.,0.,1.));
#4093=DIRECTION('ref_axis',(0.309016994374947,-0.951056516295154,0.));
#4094=DIRECTION('center_axis',(0.,0.,-1.));
#4095=DIRECTION('ref_axis',(0.309016994374946,0.951056516295154,0.));
#4096=DIRECTION('',(0.,0.,-1.));
#4097=DIRECTION('',(0.,0.,1.));
#4098=DIRECTION('center_axis',(0.,0.,1.));
#4099=DIRECTION('ref_axis',(-0.309016994374947,-0.951056516295154,0.));
#4100=DIRECTION('center_axis',(0.,0.,-1.));
#4101=DIRECTION('ref_axis',(0.809016994374947,0.587785252292474,0.));
#4102=DIRECTION('',(0.,0.,-1.));
#4103=DIRECTION('',(0.,0.,1.));
#4104=DIRECTION('center_axis',(0.,0.,1.));
#4105=DIRECTION('ref_axis',(-0.809016994374947,-0.587785252292473,0.));
#4106=DIRECTION('center_axis',(0.,0.,1.));
#4107=DIRECTION('ref_axis',(1.,0.,0.));
#4108=DIRECTION('center_axis',(0.,0.,1.));
#4109=DIRECTION('ref_axis',(1.,0.,0.));
#4110=DIRECTION('center_axis',(0.,0.,1.));
#4111=DIRECTION('ref_axis',(1.,0.,0.));
#4112=DIRECTION('center_axis',(0.,0.,1.));
#4113=DIRECTION('ref_axis',(1.,0.,0.));
#4114=DIRECTION('center_axis',(0.,0.,1.));
#4115=DIRECTION('ref_axis',(1.,0.,0.));
#4116=DIRECTION('center_axis',(0.,0.,1.));
#4117=DIRECTION('ref_axis',(1.,0.,0.));
#4118=DIRECTION('center_axis',(0.,0.,1.));
#4119=DIRECTION('ref_axis',(1.,0.,0.));
#4120=DIRECTION('center_axis',(0.,0.,1.));
#4121=DIRECTION('ref_axis',(1.,0.,0.));
#4122=DIRECTION('center_axis',(0.,0.,1.));
#4123=DIRECTION('ref_axis',(1.,0.,0.));
#4124=DIRECTION('center_axis',(0.,0.,1.));
#4125=DIRECTION('ref_axis',(1.,0.,0.));
#4126=DIRECTION('center_axis',(0.,0.,1.));
#4127=DIRECTION('ref_axis',(-1.,0.,0.));
#4128=DIRECTION('center_axis',(0.,0.,1.));
#4129=DIRECTION('ref_axis',(1.,0.,0.));
#4130=DIRECTION('center_axis',(0.,0.,1.));
#4131=DIRECTION('ref_axis',(1.,0.,0.));
#4132=DIRECTION('center_axis',(0.,0.,1.));
#4133=DIRECTION('ref_axis',(1.,0.,0.));
#4134=DIRECTION('center_axis',(0.,0.,1.));
#4135=DIRECTION('ref_axis',(1.,0.,0.));
#4136=DIRECTION('',(0.,0.,-1.));
#4137=DIRECTION('center_axis',(0.,0.,1.));
#4138=DIRECTION('ref_axis',(1.,0.,0.));
#4139=DIRECTION('center_axis',(0.,0.,1.));
#4140=DIRECTION('ref_axis',(1.,0.,0.));
#4141=DIRECTION('center_axis',(0.,0.,1.));
#4142=DIRECTION('ref_axis',(1.,0.,0.));
#4143=DIRECTION('center_axis',(0.,0.,1.));
#4144=DIRECTION('ref_axis',(1.,0.,0.));
#4145=DIRECTION('center_axis',(0.,0.,1.));
#4146=DIRECTION('ref_axis',(1.,0.,0.));
#4147=DIRECTION('center_axis',(0.,0.,1.));
#4148=DIRECTION('ref_axis',(1.,0.,0.));
#4149=DIRECTION('center_axis',(0.,0.,1.));
#4150=DIRECTION('ref_axis',(1.,0.,0.));
#4151=DIRECTION('center_axis',(0.,0.,1.));
#4152=DIRECTION('ref_axis',(1.,0.,0.));
#4153=DIRECTION('center_axis',(0.,0.,1.));
#4154=DIRECTION('ref_axis',(1.,0.,0.));
#4155=DIRECTION('center_axis',(0.,0.,1.));
#4156=DIRECTION('ref_axis',(1.,0.,0.));
#4157=DIRECTION('center_axis',(0.,0.,1.));
#4158=DIRECTION('ref_axis',(1.,0.,0.));
#4159=DIRECTION('center_axis',(0.,0.,1.));
#4160=DIRECTION('ref_axis',(1.,0.,0.));
#4161=DIRECTION('center_axis',(0.,0.,1.));
#4162=DIRECTION('ref_axis',(1.,0.,0.));
#4163=DIRECTION('center_axis',(0.,0.,1.));
#4164=DIRECTION('ref_axis',(1.,0.,0.));
#4165=DIRECTION('center_axis',(0.,0.,1.));
#4166=DIRECTION('ref_axis',(1.,0.,0.));
#4167=DIRECTION('center_axis',(0.,0.,1.));
#4168=DIRECTION('ref_axis',(1.,0.,0.));
#4169=DIRECTION('center_axis',(0.,0.,1.));
#4170=DIRECTION('ref_axis',(1.,0.,0.));
#4171=DIRECTION('center_axis',(0.,0.,-1.));
#4172=DIRECTION('ref_axis',(1.,0.,0.));
#4173=DIRECTION('center_axis',(1.22464679914735E-16,-1.,0.));
#4174=DIRECTION('ref_axis',(-1.,-1.22464679914735E-16,0.));
#4175=DIRECTION('center_axis',(0.,0.,1.));
#4176=DIRECTION('ref_axis',(1.,0.,0.));
#4177=DIRECTION('center_axis',(0.,0.,-1.));
#4178=DIRECTION('ref_axis',(1.,-1.22464679914735E-16,0.));
#4179=DIRECTION('',(0.,0.,1.));
#4180=DIRECTION('center_axis',(0.,0.,1.));
#4181=DIRECTION('ref_axis',(1.,0.,0.));
#4182=DIRECTION('center_axis',(0.,0.,1.));
#4183=DIRECTION('ref_axis',(1.,0.,0.));
#4184=DIRECTION('center_axis',(0.,0.,-1.));
#4185=DIRECTION('ref_axis',(1.,0.,0.));
#4186=DIRECTION('center_axis',(0.,0.,-1.));
#4187=DIRECTION('ref_axis',(1.,0.,0.));
#4188=DIRECTION('',(0.,0.,1.));
#4189=DIRECTION('center_axis',(0.,0.,1.));
#4190=DIRECTION('ref_axis',(1.,0.,0.));
#4191=DIRECTION('axis',(0.,0.,1.));
#4192=DIRECTION('refdir',(1.,0.,0.));
#4193=DIRECTION('center_axis',(-1.,0.,0.));
#4194=DIRECTION('ref_axis',(0.,0.968583161128631,-0.248689887164855));
#4195=DIRECTION('',(-1.,0.,0.));
#4196=DIRECTION('',(1.,0.,0.));
#4197=DIRECTION('center_axis',(-1.,0.,0.));
#4198=DIRECTION('ref_axis',(0.,0.876306680043864,-0.481753674101715));
#4199=DIRECTION('',(-1.,0.,0.));
#4200=DIRECTION('',(1.,0.,0.));
#4201=DIRECTION('center_axis',(-1.,0.,0.));
#4202=DIRECTION('ref_axis',(0.,0.728968627421412,-0.684547105928688));
#4203=DIRECTION('',(-1.,0.,0.));
#4204=DIRECTION('',(1.,0.,0.));
#4205=DIRECTION('center_axis',(-1.,0.,0.));
#4206=DIRECTION('ref_axis',(0.,0.535826794978997,-0.844327925502015));
#4207=DIRECTION('',(-1.,0.,0.));
#4208=DIRECTION('',(1.,0.,0.));
#4209=DIRECTION('center_axis',(-1.,0.,0.));
#4210=DIRECTION('ref_axis',(0.,0.309016994374947,-0.951056516295154));
#4211=DIRECTION('',(-1.,0.,0.));
#4212=DIRECTION('',(1.,0.,0.));
#4213=DIRECTION('center_axis',(-1.,0.,0.));
#4214=DIRECTION('ref_axis',(0.,0.0627905195293137,-0.998026728428272));
#4215=DIRECTION('',(-1.,0.,0.));
#4216=DIRECTION('',(1.,0.,0.));
#4217=DIRECTION('center_axis',(-1.,0.,0.));
#4218=DIRECTION('ref_axis',(0.,-0.187381314585725,-0.982287250728689));
#4219=DIRECTION('',(-1.,0.,0.));
#4220=DIRECTION('',(1.,0.,0.));
#4221=DIRECTION('center_axis',(-1.,0.,0.));
#4222=DIRECTION('ref_axis',(0.,-0.425779291565072,-0.90482705246602));
#4223=DIRECTION('',(-1.,0.,0.));
#4224=DIRECTION('',(1.,0.,0.));
#4225=DIRECTION('center_axis',(-1.,0.,0.));
#4226=DIRECTION('ref_axis',(0.,-0.637423989748689,-0.770513242775789));
#4227=DIRECTION('',(-1.,0.,0.));
#4228=DIRECTION('',(1.,0.,0.));
#4229=DIRECTION('center_axis',(-1.,0.,0.));
#4230=DIRECTION('ref_axis',(0.,-0.809016994374947,-0.587785252292473));
#4231=DIRECTION('',(-1.,0.,0.));
#4232=DIRECTION('',(1.,0.,0.));
#4233=DIRECTION('center_axis',(-1.,0.,0.));
#4234=DIRECTION('ref_axis',(0.,-0.929776485888251,-0.368124552684678));
#4235=DIRECTION('',(-1.,0.,0.));
#4236=DIRECTION('',(1.,0.,0.));
#4237=DIRECTION('center_axis',(-1.,0.,0.));
#4238=DIRECTION('ref_axis',(0.,-0.992114701314478,-0.125333233564304));
#4239=DIRECTION('',(-1.,0.,0.));
#4240=DIRECTION('',(1.,0.,0.));
#4241=DIRECTION('center_axis',(-1.,0.,0.));
#4242=DIRECTION('ref_axis',(0.,-0.992114701314478,0.125333233564304));
#4243=DIRECTION('',(-1.,0.,0.));
#4244=DIRECTION('',(1.,0.,0.));
#4245=DIRECTION('center_axis',(-1.,0.,0.));
#4246=DIRECTION('ref_axis',(0.,-0.929776485888251,0.368124552684678));
#4247=DIRECTION('',(-1.,0.,0.));
#4248=DIRECTION('',(1.,0.,0.));
#4249=DIRECTION('center_axis',(-1.,0.,0.));
#4250=DIRECTION('ref_axis',(0.,-0.809016994374947,0.587785252292473));
#4251=DIRECTION('',(-1.,0.,0.));
#4252=DIRECTION('',(1.,0.,0.));
#4253=DIRECTION('center_axis',(-1.,0.,0.));
#4254=DIRECTION('ref_axis',(0.,-0.63742398974869,0.770513242775789));
#4255=DIRECTION('',(-1.,0.,0.));
#4256=DIRECTION('',(1.,0.,0.));
#4257=DIRECTION('center_axis',(-1.,0.,0.));
#4258=DIRECTION('ref_axis',(0.,-0.425779291565073,0.904827052466019));
#4259=DIRECTION('',(-1.,0.,0.));
#4260=DIRECTION('',(1.,0.,0.));
#4261=DIRECTION('center_axis',(-1.,0.,0.));
#4262=DIRECTION('ref_axis',(0.,-0.187381314585725,0.982287250728689));
#4263=DIRECTION('',(-1.,0.,0.));
#4264=DIRECTION('',(1.,0.,0.));
#4265=DIRECTION('center_axis',(-1.,0.,0.));
#4266=DIRECTION('ref_axis',(0.,0.0627905195293132,0.998026728428272));
#4267=DIRECTION('',(-1.,0.,0.));
#4268=DIRECTION('',(1.,0.,0.));
#4269=DIRECTION('center_axis',(-1.,0.,0.));
#4270=DIRECTION('ref_axis',(0.,0.309016994374947,0.951056516295154));
#4271=DIRECTION('',(-1.,0.,0.));
#4272=DIRECTION('',(1.,0.,0.));
#4273=DIRECTION('center_axis',(-1.,0.,0.));
#4274=DIRECTION('ref_axis',(0.,0.535826794978997,0.844327925502015));
#4275=DIRECTION('',(-1.,0.,0.));
#4276=DIRECTION('',(1.,0.,0.));
#4277=DIRECTION('center_axis',(-1.,0.,0.));
#4278=DIRECTION('ref_axis',(0.,0.728968627421412,0.684547105928689));
#4279=DIRECTION('',(-1.,0.,0.));
#4280=DIRECTION('',(1.,0.,0.));
#4281=DIRECTION('center_axis',(-1.,0.,0.));
#4282=DIRECTION('ref_axis',(0.,0.876306680043864,0.481753674101715));
#4283=DIRECTION('',(-1.,0.,0.));
#4284=DIRECTION('',(1.,0.,0.));
#4285=DIRECTION('center_axis',(-1.,0.,0.));
#4286=DIRECTION('ref_axis',(0.,0.968583161128631,0.248689887164855));
#4287=DIRECTION('',(-1.,0.,0.));
#4288=DIRECTION('',(1.,0.,0.));
#4289=DIRECTION('center_axis',(-1.,0.,0.));
#4290=DIRECTION('ref_axis',(0.,0.,-1.));
#4291=DIRECTION('center_axis',(1.,0.,0.));
#4292=DIRECTION('ref_axis',(0.,0.,-1.));
#4293=DIRECTION('',(-0.705535732530397,-8.67875770714651E-17,0.708674347018993));
#4294=DIRECTION('center_axis',(1.,0.,0.));
#4295=DIRECTION('ref_axis',(0.,0.,-1.));
#4296=DIRECTION('center_axis',(1.,0.,0.));
#4297=DIRECTION('ref_axis',(0.,0.,-1.));
#4298=DIRECTION('center_axis',(1.,0.,0.));
#4299=DIRECTION('ref_axis',(0.,0.,-1.));
#4300=DIRECTION('center_axis',(1.,0.,0.));
#4301=DIRECTION('ref_axis',(0.,0.,-1.));
#4302=DIRECTION('center_axis',(1.,0.,0.));
#4303=DIRECTION('ref_axis',(0.,0.,-1.));
#4304=DIRECTION('center_axis',(1.,0.,0.));
#4305=DIRECTION('ref_axis',(0.,0.,-1.));
#4306=DIRECTION('center_axis',(1.,0.,0.));
#4307=DIRECTION('ref_axis',(0.,0.,-1.));
#4308=DIRECTION('center_axis',(1.,0.,0.));
#4309=DIRECTION('ref_axis',(0.,0.,-1.));
#4310=DIRECTION('center_axis',(1.,0.,0.));
#4311=DIRECTION('ref_axis',(0.,0.,-1.));
#4312=DIRECTION('center_axis',(1.,0.,0.));
#4313=DIRECTION('ref_axis',(0.,0.,-1.));
#4314=DIRECTION('center_axis',(1.,0.,0.));
#4315=DIRECTION('ref_axis',(0.,0.,-1.));
#4316=DIRECTION('center_axis',(1.,0.,0.));
#4317=DIRECTION('ref_axis',(0.,0.,-1.));
#4318=DIRECTION('center_axis',(1.,0.,0.));
#4319=DIRECTION('ref_axis',(0.,0.,-1.));
#4320=DIRECTION('center_axis',(1.,0.,0.));
#4321=DIRECTION('ref_axis',(0.,0.,-1.));
#4322=DIRECTION('center_axis',(1.,0.,0.));
#4323=DIRECTION('ref_axis',(0.,0.,-1.));
#4324=DIRECTION('center_axis',(1.,0.,0.));
#4325=DIRECTION('ref_axis',(0.,0.,-1.));
#4326=DIRECTION('center_axis',(1.,0.,0.));
#4327=DIRECTION('ref_axis',(0.,0.,-1.));
#4328=DIRECTION('center_axis',(1.,0.,0.));
#4329=DIRECTION('ref_axis',(0.,0.,-1.));
#4330=DIRECTION('center_axis',(1.,0.,0.));
#4331=DIRECTION('ref_axis',(0.,0.,-1.));
#4332=DIRECTION('center_axis',(1.,0.,0.));
#4333=DIRECTION('ref_axis',(0.,0.,-1.));
#4334=DIRECTION('center_axis',(1.,0.,0.));
#4335=DIRECTION('ref_axis',(0.,0.,-1.));
#4336=DIRECTION('center_axis',(1.,0.,0.));
#4337=DIRECTION('ref_axis',(0.,0.,-1.));
#4338=DIRECTION('center_axis',(1.,0.,0.));
#4339=DIRECTION('ref_axis',(0.,0.,-1.));
#4340=DIRECTION('center_axis',(1.,0.,0.));
#4341=DIRECTION('ref_axis',(0.,0.,-1.));
#4342=DIRECTION('center_axis',(1.,0.,0.));
#4343=DIRECTION('ref_axis',(0.,0.,-1.));
#4344=DIRECTION('center_axis',(1.,0.,0.));
#4345=DIRECTION('ref_axis',(0.,0.,-1.));
#4346=DIRECTION('center_axis',(1.,0.,0.));
#4347=DIRECTION('ref_axis',(0.,0.,-1.));
#4348=DIRECTION('',(1.,0.,0.));
#4349=DIRECTION('center_axis',(1.,0.,0.));
#4350=DIRECTION('ref_axis',(0.,0.,-1.));
#4351=DIRECTION('',(-1.,0.,0.));
#4352=DIRECTION('center_axis',(1.,0.,0.));
#4353=DIRECTION('ref_axis',(0.,0.,-1.));
#4354=DIRECTION('center_axis',(1.,0.,0.));
#4355=DIRECTION('ref_axis',(0.,0.,-1.));
#4356=DIRECTION('center_axis',(1.,0.,0.));
#4357=DIRECTION('ref_axis',(0.,0.,-1.));
#4358=DIRECTION('center_axis',(1.,0.,0.));
#4359=DIRECTION('ref_axis',(0.,0.,-1.));
#4360=DIRECTION('center_axis',(1.,0.,0.));
#4361=DIRECTION('ref_axis',(0.,0.,-1.));
#4362=DIRECTION('center_axis',(1.,0.,0.));
#4363=DIRECTION('ref_axis',(0.,0.,-1.));
#4364=DIRECTION('center_axis',(1.,0.,0.));
#4365=DIRECTION('ref_axis',(0.,0.,-1.));
#4366=DIRECTION('center_axis',(1.,0.,0.));
#4367=DIRECTION('ref_axis',(0.,0.,-1.));
#4368=DIRECTION('center_axis',(1.,0.,0.));
#4369=DIRECTION('ref_axis',(0.,0.,-1.));
#4370=DIRECTION('center_axis',(1.,0.,0.));
#4371=DIRECTION('ref_axis',(0.,0.,-1.));
#4372=DIRECTION('center_axis',(1.,0.,0.));
#4373=DIRECTION('ref_axis',(0.,0.,-1.));
#4374=DIRECTION('center_axis',(1.,0.,0.));
#4375=DIRECTION('ref_axis',(0.,0.,-1.));
#4376=DIRECTION('center_axis',(1.,0.,0.));
#4377=DIRECTION('ref_axis',(0.,0.,-1.));
#4378=DIRECTION('center_axis',(1.,0.,0.));
#4379=DIRECTION('ref_axis',(0.,0.,-1.));
#4380=DIRECTION('center_axis',(1.,0.,0.));
#4381=DIRECTION('ref_axis',(0.,0.,-1.));
#4382=DIRECTION('center_axis',(1.,0.,0.));
#4383=DIRECTION('ref_axis',(0.,0.,-1.));
#4384=DIRECTION('center_axis',(1.,0.,0.));
#4385=DIRECTION('ref_axis',(0.,0.,-1.));
#4386=DIRECTION('center_axis',(1.,0.,0.));
#4387=DIRECTION('ref_axis',(0.,0.,-1.));
#4388=DIRECTION('center_axis',(1.,0.,0.));
#4389=DIRECTION('ref_axis',(0.,0.,-1.));
#4390=DIRECTION('center_axis',(1.,0.,0.));
#4391=DIRECTION('ref_axis',(0.,0.,-1.));
#4392=DIRECTION('center_axis',(1.,0.,0.));
#4393=DIRECTION('ref_axis',(0.,0.,-1.));
#4394=DIRECTION('center_axis',(1.,0.,0.));
#4395=DIRECTION('ref_axis',(0.,0.,-1.));
#4396=DIRECTION('center_axis',(1.,0.,0.));
#4397=DIRECTION('ref_axis',(0.,0.,-1.));
#4398=DIRECTION('center_axis',(1.,0.,0.));
#4399=DIRECTION('ref_axis',(0.,0.,-1.));
#4400=DIRECTION('center_axis',(1.,0.,0.));
#4401=DIRECTION('ref_axis',(0.,0.,-1.));
#4402=DIRECTION('center_axis',(1.,0.,0.));
#4403=DIRECTION('ref_axis',(0.,0.,-1.));
#4404=DIRECTION('center_axis',(1.,0.,0.));
#4405=DIRECTION('ref_axis',(0.,0.,-1.));
#4406=DIRECTION('center_axis',(1.,0.,0.));
#4407=DIRECTION('ref_axis',(0.,0.,-1.));
#4408=DIRECTION('center_axis',(1.,0.,0.));
#4409=DIRECTION('ref_axis',(0.,0.,-1.));
#4410=DIRECTION('center_axis',(1.,0.,0.));
#4411=DIRECTION('ref_axis',(0.,0.,-1.));
#4412=DIRECTION('center_axis',(1.,0.,0.));
#4413=DIRECTION('ref_axis',(0.,0.,-1.));
#4414=DIRECTION('center_axis',(1.,0.,0.));
#4415=DIRECTION('ref_axis',(0.,0.,-1.));
#4416=DIRECTION('center_axis',(1.,0.,0.));
#4417=DIRECTION('ref_axis',(0.,0.,-1.));
#4418=DIRECTION('center_axis',(1.,0.,0.));
#4419=DIRECTION('ref_axis',(0.,0.,-1.));
#4420=DIRECTION('center_axis',(1.,0.,0.));
#4421=DIRECTION('ref_axis',(0.,0.,-1.));
#4422=DIRECTION('center_axis',(1.,0.,0.));
#4423=DIRECTION('ref_axis',(0.,0.,-1.));
#4424=DIRECTION('center_axis',(1.,0.,0.));
#4425=DIRECTION('ref_axis',(0.,0.,-1.));
#4426=DIRECTION('center_axis',(1.,0.,0.));
#4427=DIRECTION('ref_axis',(0.,0.,-1.));
#4428=DIRECTION('center_axis',(1.,0.,0.));
#4429=DIRECTION('ref_axis',(0.,0.,-1.));
#4430=DIRECTION('center_axis',(1.,0.,0.));
#4431=DIRECTION('ref_axis',(0.,0.,-1.));
#4432=DIRECTION('center_axis',(1.,0.,0.));
#4433=DIRECTION('ref_axis',(0.,0.,-1.));
#4434=DIRECTION('center_axis',(1.,0.,0.));
#4435=DIRECTION('ref_axis',(0.,0.,-1.));
#4436=DIRECTION('center_axis',(1.,0.,0.));
#4437=DIRECTION('ref_axis',(0.,0.,-1.));
#4438=DIRECTION('center_axis',(1.,0.,0.));
#4439=DIRECTION('ref_axis',(0.,0.,-1.));
#4440=DIRECTION('center_axis',(1.,0.,0.));
#4441=DIRECTION('ref_axis',(0.,0.,-1.));
#4442=DIRECTION('center_axis',(-1.,0.,0.));
#4443=DIRECTION('ref_axis',(0.,1.,0.));
#4444=DIRECTION('center_axis',(1.,0.,0.));
#4445=DIRECTION('ref_axis',(0.,0.,-1.));
#4446=DIRECTION('center_axis',(1.,0.,0.));
#4447=DIRECTION('ref_axis',(0.,0.,-1.));
#4448=DIRECTION('',(-1.,0.,0.));
#4449=DIRECTION('center_axis',(1.,0.,0.));
#4450=DIRECTION('ref_axis',(0.,0.,-1.));
#4451=DIRECTION('center_axis',(-1.,0.,0.));
#4452=DIRECTION('ref_axis',(0.,0.,1.));
#4453=DIRECTION('center_axis',(1.,0.,0.));
#4454=DIRECTION('ref_axis',(0.,0.,-1.));
#4455=DIRECTION('center_axis',(1.,0.,0.));
#4456=DIRECTION('ref_axis',(0.,0.,-1.));
#4457=DIRECTION('center_axis',(1.,0.,0.));
#4458=DIRECTION('ref_axis',(0.,0.,-1.));
#4459=DIRECTION('',(-1.,0.,0.));
#4460=DIRECTION('center_axis',(1.,0.,0.));
#4461=DIRECTION('ref_axis',(0.,0.,-1.));
#4462=DIRECTION('center_axis',(1.,0.,0.));
#4463=DIRECTION('ref_axis',(0.,0.,-1.));
#4464=DIRECTION('',(-0.708674347018993,8.64032076527434E-17,-0.705535732530397));
#4465=DIRECTION('center_axis',(1.,0.,0.));
#4466=DIRECTION('ref_axis',(0.,0.,-1.));
#4467=DIRECTION('axis',(0.,0.,1.));
#4468=DIRECTION('refdir',(1.,0.,0.));
#4469=DIRECTION('center_axis',(-1.,0.,0.));
#4470=DIRECTION('ref_axis',(0.,-1.,0.));
#4471=DIRECTION('center_axis',(1.,0.,0.));
#4472=DIRECTION('ref_axis',(0.,0.,-1.));
#4473=DIRECTION('center_axis',(1.,0.,0.));
#4474=DIRECTION('ref_axis',(0.,0.,-1.));
#4475=DIRECTION('',(-1.,0.,0.));
#4476=DIRECTION('center_axis',(1.,0.,0.));
#4477=DIRECTION('ref_axis',(0.,0.,-1.));
#4478=DIRECTION('center_axis',(1.,0.,0.));
#4479=DIRECTION('ref_axis',(0.,0.,-1.));
#4480=DIRECTION('',(-1.,0.,0.));
#4481=DIRECTION('',(1.,0.,0.));
#4482=DIRECTION('center_axis',(0.,1.,0.));
#4483=DIRECTION('ref_axis',(-1.,0.,0.));
#4484=DIRECTION('',(0.,0.,1.));
#4485=DIRECTION('',(1.,0.,0.));
#4486=DIRECTION('',(0.,0.,1.));
#4487=DIRECTION('center_axis',(0.,0.,1.));
#4488=DIRECTION('ref_axis',(0.,-1.,0.));
#4489=DIRECTION('',(0.,0.,1.));
#4490=DIRECTION('center_axis',(0.,0.,-1.));
#4491=DIRECTION('ref_axis',(1.,0.,0.));
#4492=DIRECTION('',(0.,0.,-1.));
#4493=DIRECTION('center_axis',(0.,0.,-1.));
#4494=DIRECTION('ref_axis',(1.,0.,0.));
#4495=DIRECTION('center_axis',(0.,0.,1.));
#4496=DIRECTION('ref_axis',(1.,0.,0.));
#4497=DIRECTION('center_axis',(0.,-1.,0.));
#4498=DIRECTION('ref_axis',(1.,0.,0.));
#4499=DIRECTION('',(0.,0.,1.));
#4500=DIRECTION('',(-1.,0.,0.));
#4501=DIRECTION('center_axis',(0.,0.,1.));
#4502=DIRECTION('ref_axis',(0.,1.,0.));
#4503=DIRECTION('center_axis',(1.,0.,0.));
#4504=DIRECTION('ref_axis',(0.,0.,1.));
#4505=DIRECTION('center_axis',(-1.,0.,0.));
#4506=DIRECTION('ref_axis',(0.,0.,1.));
#4507=DIRECTION('center_axis',(-1.,0.,0.));
#4508=DIRECTION('ref_axis',(0.,0.,1.));
#4509=DIRECTION('',(-0.707106781186548,-8.65956056235493E-17,0.707106781186548));
#4510=DIRECTION('center_axis',(1.,0.,0.));
#4511=DIRECTION('ref_axis',(0.,0.,1.));
#4512=DIRECTION('center_axis',(-1.,0.,0.));
#4513=DIRECTION('ref_axis',(0.,0.,1.));
#4514=DIRECTION('center_axis',(1.,0.,0.));
#4515=DIRECTION('ref_axis',(0.,0.,-1.));
#4516=DIRECTION('center_axis',(1.,0.,0.));
#4517=DIRECTION('ref_axis',(0.,0.,-1.));
#4518=DIRECTION('center_axis',(1.,0.,0.));
#4519=DIRECTION('ref_axis',(0.,0.,-1.));
#4520=DIRECTION('',(-1.,0.,0.));
#4521=DIRECTION('center_axis',(1.,0.,0.));
#4522=DIRECTION('ref_axis',(0.,0.,-1.));
#4523=DIRECTION('center_axis',(-1.,0.,0.));
#4524=DIRECTION('ref_axis',(0.,1.22464679914735E-16,1.));
#4525=DIRECTION('center_axis',(0.,-1.,-1.22464679914735E-16));
#4526=DIRECTION('ref_axis',(0.,-1.22464679914735E-16,1.));
#4527=DIRECTION('center_axis',(1.,0.,0.));
#4528=DIRECTION('ref_axis',(0.,1.22464679914735E-16,1.));
#4529=DIRECTION('center_axis',(1.,0.,0.));
#4530=DIRECTION('ref_axis',(0.,0.,-1.));
#4531=DIRECTION('',(-1.,0.,0.));
#4532=DIRECTION('',(-1.,0.,0.));
#4533=DIRECTION('',(-1.,0.,0.));
#4534=DIRECTION('center_axis',(-1.,0.,0.));
#4535=DIRECTION('ref_axis',(0.,1.22464679914735E-16,1.));
#4536=DIRECTION('center_axis',(1.,0.,0.));
#4537=DIRECTION('ref_axis',(0.,0.,-1.));
#4538=DIRECTION('center_axis',(1.,0.,0.));
#4539=DIRECTION('ref_axis',(0.,0.,-1.));
#4540=DIRECTION('center_axis',(0.,-1.,-1.22464679914735E-16));
#4541=DIRECTION('ref_axis',(0.,-1.22464679914735E-16,1.));
#4542=DIRECTION('center_axis',(1.,0.,0.));
#4543=DIRECTION('ref_axis',(0.,1.22464679914735E-16,1.));
#4544=DIRECTION('center_axis',(-1.,0.,0.));
#4545=DIRECTION('ref_axis',(0.,0.,1.));
#4546=DIRECTION('center_axis',(1.,0.,0.));
#4547=DIRECTION('ref_axis',(0.,0.,-1.));
#4548=DIRECTION('center_axis',(1.,0.,0.));
#4549=DIRECTION('ref_axis',(0.,0.,-1.));
#4550=DIRECTION('center_axis',(1.,0.,0.));
#4551=DIRECTION('ref_axis',(0.,0.,-1.));
#4552=DIRECTION('',(-1.,0.,0.));
#4553=DIRECTION('axis',(0.,0.,1.));
#4554=DIRECTION('refdir',(1.,0.,0.));
#4555=DIRECTION('center_axis',(0.,0.,1.));
#4556=DIRECTION('ref_axis',(1.,0.,0.));
#4557=DIRECTION('center_axis',(1.,0.,0.));
#4558=DIRECTION('ref_axis',(0.,0.,-1.));
#4559=DIRECTION('center_axis',(-1.22464679914735E-16,1.,0.));
#4560=DIRECTION('ref_axis',(-1.,-1.22464679914735E-16,0.));
#4561=DIRECTION('center_axis',(1.,0.,0.));
#4562=DIRECTION('ref_axis',(0.,0.,-1.));
#4563=DIRECTION('center_axis',(-1.22464679914735E-16,1.,0.));
#4564=DIRECTION('ref_axis',(-1.,-1.22464679914735E-16,0.));
#4565=DIRECTION('center_axis',(1.,0.,0.));
#4566=DIRECTION('ref_axis',(0.,0.,-1.));
#4567=DIRECTION('center_axis',(1.,0.,0.));
#4568=DIRECTION('ref_axis',(0.,0.,-1.));
#4569=DIRECTION('center_axis',(1.,0.,0.));
#4570=DIRECTION('ref_axis',(0.,0.,-1.));
#4571=DIRECTION('center_axis',(1.,0.,0.));
#4572=DIRECTION('ref_axis',(0.,0.,-1.));
#4573=DIRECTION('center_axis',(1.,0.,0.));
#4574=DIRECTION('ref_axis',(0.,0.,-1.));
#4575=DIRECTION('',(-1.,0.,0.));
#4576=DIRECTION('axis',(0.,0.,1.));
#4577=DIRECTION('refdir',(1.,0.,0.));
#4578=DIRECTION('center_axis',(1.,0.,0.));
#4579=DIRECTION('ref_axis',(0.,-1.,0.));
#4580=DIRECTION('center_axis',(1.,0.,0.));
#4581=DIRECTION('ref_axis',(0.,-1.,0.));
#4582=DIRECTION('',(0.707106781186548,0.707106781186547,-8.65956056235493E-17));
#4583=DIRECTION('center_axis',(-1.,0.,0.));
#4584=DIRECTION('ref_axis',(0.,-1.,0.));
#4585=DIRECTION('center_axis',(-1.,0.,0.));
#4586=DIRECTION('ref_axis',(0.,-1.,0.));
#4587=DIRECTION('center_axis',(1.,0.,0.));
#4588=DIRECTION('ref_axis',(0.,0.,-1.));
#4589=DIRECTION('center_axis',(1.,0.,0.));
#4590=DIRECTION('ref_axis',(0.,-1.,0.));
#4591=DIRECTION('center_axis',(1.,0.,0.));
#4592=DIRECTION('ref_axis',(0.,-1.,0.));
#4593=DIRECTION('',(-1.,0.,0.));
#4594=DIRECTION('center_axis',(1.,0.,0.));
#4595=DIRECTION('ref_axis',(0.,0.,-1.));
#4596=DIRECTION('center_axis',(1.,0.,0.));
#4597=DIRECTION('ref_axis',(0.,0.,-1.));
#4598=DIRECTION('center_axis',(1.,0.,0.));
#4599=DIRECTION('ref_axis',(0.,0.,-1.));
#4600=DIRECTION('',(1.,0.,0.));
#4601=DIRECTION('center_axis',(-1.,0.,0.));
#4602=DIRECTION('ref_axis',(0.,-1.,0.));
#4603=DIRECTION('axis',(0.,0.,1.));
#4604=DIRECTION('refdir',(1.,0.,0.));
#4605=DIRECTION('center_axis',(0.,0.,1.));
#4606=DIRECTION('ref_axis',(1.,0.,0.));
#4607=DIRECTION('center_axis',(1.22464679914735E-16,-1.,0.));
#4608=DIRECTION('ref_axis',(-1.,-1.22464679914735E-16,0.));
#4609=DIRECTION('axis',(0.,0.,1.));
#4610=DIRECTION('refdir',(1.,0.,0.));
#4611=DIRECTION('center_axis',(1.,0.,0.));
#4612=DIRECTION('ref_axis',(0.,1.,0.));
#4613=DIRECTION('center_axis',(1.,0.,0.));
#4614=DIRECTION('ref_axis',(0.,1.,0.));
#4615=DIRECTION('',(-1.,0.,0.));
#4616=DIRECTION('center_axis',(1.,0.,0.));
#4617=DIRECTION('ref_axis',(0.,1.,0.));
#4618=DIRECTION('center_axis',(1.,0.,0.));
#4619=DIRECTION('ref_axis',(0.,1.,0.));
#4620=DIRECTION('center_axis',(1.,0.,0.));
#4621=DIRECTION('ref_axis',(0.,1.,0.));
#4622=DIRECTION('axis',(0.,0.,1.));
#4623=DIRECTION('refdir',(1.,0.,0.));
#4624=DIRECTION('center_axis',(-1.,0.,0.));
#4625=DIRECTION('ref_axis',(0.,-1.,0.));
#4626=DIRECTION('center_axis',(1.,0.,0.));
#4627=DIRECTION('ref_axis',(0.,-1.,0.));
#4628=DIRECTION('',(1.,0.,0.));
#4629=DIRECTION('center_axis',(1.,0.,0.));
#4630=DIRECTION('ref_axis',(0.,-1.,0.));
#4631=DIRECTION('center_axis',(-1.,0.,0.));
#4632=DIRECTION('ref_axis',(0.,-1.,0.));
#4633=DIRECTION('center_axis',(-1.,0.,0.));
#4634=DIRECTION('ref_axis',(0.,-1.,0.));
#4635=DIRECTION('',(1.,0.,0.));
#4636=DIRECTION('center_axis',(-1.,0.,0.));
#4637=DIRECTION('ref_axis',(0.,-1.,0.));
#4638=DIRECTION('center_axis',(-1.,0.,0.));
#4639=DIRECTION('ref_axis',(0.,-1.,0.));
#4640=DIRECTION('center_axis',(-1.,0.,0.));
#4641=DIRECTION('ref_axis',(0.,-1.,0.));
#4642=DIRECTION('',(0.,0.,1.));
#4643=DIRECTION('',(1.,0.,0.));
#4644=DIRECTION('',(0.,0.,1.));
#4645=DIRECTION('',(1.,0.,0.));
#4646=DIRECTION('',(0.,0.,1.));
#4647=DIRECTION('',(1.,0.,0.));
#4648=DIRECTION('',(0.,0.,1.));
#4649=DIRECTION('',(1.,0.,0.));
#4650=DIRECTION('',(0.,0.,1.));
#4651=DIRECTION('',(1.,0.,0.));
#4652=DIRECTION('',(0.,0.,1.));
#4653=DIRECTION('',(1.,0.,0.));
#4654=DIRECTION('',(0.,0.,1.));
#4655=DIRECTION('',(1.,0.,0.));
#4656=DIRECTION('',(0.,0.,1.));
#4657=DIRECTION('',(1.,0.,0.));
#4658=DIRECTION('',(0.,0.,1.));
#4659=DIRECTION('',(1.,0.,0.));
#4660=DIRECTION('',(0.,0.,1.));
#4661=DIRECTION('',(1.,0.,0.));
#4662=CARTESIAN_POINT('',(0.,0.,0.));
#4663=CARTESIAN_POINT('',(0.,0.,0.));
#4664=CARTESIAN_POINT('Origin',(50.5120935137584,0.,0.));
#4665=CARTESIAN_POINT('',(50.5120935137584,-1.28658893794659E-15,10.5057959473896));
#4666=CARTESIAN_POINT('Origin',(50.5120935137584,0.,0.));
#4667=CARTESIAN_POINT('',(50.0120935137584,-1.22535659798922E-15,10.0057959473896));
#4668=CARTESIAN_POINT('Origin',(50.5120935137584,-1.22535659798922E-15,
10.0057959473896));
#4669=CARTESIAN_POINT('Origin',(50.0120935137584,0.,0.));
#4670=CARTESIAN_POINT('Origin',(50.0120935137584,0.,-10.5057959473896));
#4671=CARTESIAN_POINT('',(50.0120935137584,-1.16412425803185E-15,9.50579594738959));
#4672=CARTESIAN_POINT('Origin',(50.0120935137584,0.,0.));
#4673=CARTESIAN_POINT('Origin',(54.0077062393936,0.,0.));
#4674=CARTESIAN_POINT('',(58.0033189650289,-1.28658893794659E-15,10.5057959473896));
#4675=CARTESIAN_POINT('Origin',(58.0033189650289,0.,0.));
#4676=CARTESIAN_POINT('',(54.0077062393936,-1.28658893794659E-15,10.5057959473896));
#4677=CARTESIAN_POINT('Origin',(65.0333054217745,2.89627205572787,11.2802348949791));
#4678=CARTESIAN_POINT('',(58.5152881956451,1.99731386475336,10.8422004546896));
#4679=CARTESIAN_POINT('',(58.5152881956451,3.47301042256638,10.4633059774983));
#4680=CARTESIAN_POINT('Ctrl Pts',(58.5152881956451,1.99731386475335,10.8422004546895));
#4681=CARTESIAN_POINT('Ctrl Pts',(58.4654152249681,2.02482541039242,10.7857397588542));
#4682=CARTESIAN_POINT('Ctrl Pts',(58.4186772780868,2.05797507265433,10.7312801542195));
#4683=CARTESIAN_POINT('Ctrl Pts',(58.3120945049187,2.15482072622166,10.6021965229197));
#4684=CARTESIAN_POINT('Ctrl Pts',(58.2507030237862,2.23349798161002,10.5226028552003));
#4685=CARTESIAN_POINT('Ctrl Pts',(58.1653214105115,2.42316764831179,10.3917259702023));
#4686=CARTESIAN_POINT('Ctrl Pts',(58.1417842183134,2.5345267480614,10.3406794321384));
#4687=CARTESIAN_POINT('Ctrl Pts',(58.1417842183134,2.76063758906463,10.2826240355627));
#4688=CARTESIAN_POINT('Ctrl Pts',(58.1653214105115,2.88281416932137,10.2737088024122));
#4689=CARTESIAN_POINT('Ctrl Pts',(58.2507030237862,3.11207338545657,10.2970230322));
#4690=CARTESIAN_POINT('Ctrl Pts',(58.3120945049187,3.21936333178,10.3288684380602));
#4691=CARTESIAN_POINT('Ctrl Pts',(58.4186772780868,3.36641633857932,10.3953295370257));
#4692=CARTESIAN_POINT('Ctrl Pts',(58.4654152249681,3.4217017236835,10.4270828807697));
#4693=CARTESIAN_POINT('Ctrl Pts',(58.5152881956451,3.47301042256638,10.4633059774983));
#4694=CARTESIAN_POINT('',(64.5333054217746,1.99731386475336,10.8422004546896));
#4695=CARTESIAN_POINT('',(65.0333054217745,1.99731386475335,10.8422004546896));
#4696=CARTESIAN_POINT('',(64.5333054217746,3.47301042256638,10.4633059774983));
#4697=CARTESIAN_POINT('Ctrl Pts',(64.5333054217746,3.47301042256638,10.4633059774983));
#4698=CARTESIAN_POINT('Ctrl Pts',(64.5841440169343,3.42140080495871,10.4268704371039));
#4699=CARTESIAN_POINT('Ctrl Pts',(64.6317941862906,3.36574304661788,10.3949381862959));
#4700=CARTESIAN_POINT('Ctrl Pts',(64.7397191574786,3.21851020835991,10.328616066089));
#4701=CARTESIAN_POINT('Ctrl Pts',(64.8016959801978,3.11150967133897,10.2969249363867));
#4702=CARTESIAN_POINT('Ctrl Pts',(64.8879780992218,2.88267500902188,10.2737355458811));
#4703=CARTESIAN_POINT('Ctrl Pts',(64.911821119031,2.76062757856656,10.2826266058217));
#4704=CARTESIAN_POINT('Ctrl Pts',(64.911821119031,2.53453675855947,10.3406768618793));
#4705=CARTESIAN_POINT('Ctrl Pts',(64.8879780992218,2.42330247917621,10.3916823646972));
#4706=CARTESIAN_POINT('Ctrl Pts',(64.8016959801978,2.23394471003842,10.5222453218365));
#4707=CARTESIAN_POINT('Ctrl Pts',(64.7397191574786,2.15544674284921,10.6015643723334));
#4708=CARTESIAN_POINT('Ctrl Pts',(64.6317941862906,2.05837654824586,10.7306128500846));
#4709=CARTESIAN_POINT('Ctrl Pts',(64.5841440169343,2.0249867619646,10.7854086243495));
#4710=CARTESIAN_POINT('Ctrl Pts',(64.5333054217746,1.99731386475335,10.8422004546895));
#4711=CARTESIAN_POINT('',(65.0333054217745,3.47301042256639,10.4633059774983));
#4712=CARTESIAN_POINT('Origin',(65.0333054217745,5.61056068645085,10.2055720021147));
#4713=CARTESIAN_POINT('',(58.5152881956451,4.63091018458434,10.0048610303352));
#4714=CARTESIAN_POINT('',(58.5152881956451,5.96601779663743,9.270879409431));
#4715=CARTESIAN_POINT('Ctrl Pts',(58.5152881956451,4.63091018458433,10.0048610303352));
#4716=CARTESIAN_POINT('Ctrl Pts',(58.4654152249681,4.64351620035041,9.94333230790271));
#4717=CARTESIAN_POINT('Ctrl Pts',(58.4186772780868,4.66208085208276,9.88233966612439));
#4718=CARTESIAN_POINT('Ctrl Pts',(58.3120945049187,4.72378212765379,9.73322689981203));
#4719=CARTESIAN_POINT('Ctrl Pts',(58.2507030237862,4.78019345214259,9.63656757576151));
#4720=CARTESIAN_POINT('Ctrl Pts',(58.1653214105115,4.93135653972417,9.46263350076087));
#4721=CARTESIAN_POINT('Ctrl Pts',(58.1417842183134,5.02652233078881,9.38549680160669));
#4722=CARTESIAN_POINT('Ctrl Pts',(58.1417842183134,5.23109169390945,9.273033842535));
#4723=CARTESIAN_POINT('Ctrl Pts',(58.1653214105115,5.34721274390418,9.23401461786969));
#4724=CARTESIAN_POINT('Ctrl Pts',(58.2507030237862,5.57506737336155,9.19958193966468));
#4725=CARTESIAN_POINT('Ctrl Pts',(58.3120945049187,5.6869062391189,9.20374493889506));
#4726=CARTESIAN_POINT('Ctrl Pts',(58.4186772780868,5.84586750850063,9.23154744455494));
#4727=CARTESIAN_POINT('Ctrl Pts',(58.4654152249681,5.90731273704185,9.24855428243148));
#4728=CARTESIAN_POINT('Ctrl Pts',(58.5152881956451,5.96601779663743,9.270879409431));
#4729=CARTESIAN_POINT('',(64.5333054217746,4.63091018458434,10.0048610303352));
#4730=CARTESIAN_POINT('',(65.0333054217746,4.63091018458433,10.0048610303352));
#4731=CARTESIAN_POINT('',(64.5333054217746,5.96601779663743,9.270879409431));
#4732=CARTESIAN_POINT('Ctrl Pts',(64.5333054217746,5.96601779663743,9.270879409431));
#4733=CARTESIAN_POINT('Ctrl Pts',(64.5841440169343,5.90696843964088,9.24842334851786));
#4734=CARTESIAN_POINT('Ctrl Pts',(64.6317941862906,5.84511804427544,9.23133582972996));
#4735=CARTESIAN_POINT('Ctrl Pts',(64.7397191574786,5.68601715578279,9.20371265882047));
#4736=CARTESIAN_POINT('Ctrl Pts',(64.8016959801978,5.5744969739228,9.19962711571201));
#4737=CARTESIAN_POINT('Ctrl Pts',(64.8879780992218,5.34708460641165,9.23407512890248));
#4738=CARTESIAN_POINT('Ctrl Pts',(64.9118211190309,5.23108263710702,9.27303882155427));
#4739=CARTESIAN_POINT('Ctrl Pts',(64.9118211190309,5.02653138759124,9.38549182258742));
#4740=CARTESIAN_POINT('Ctrl Pts',(64.8879780992218,4.9314762903809,9.46255773413038));
#4741=CARTESIAN_POINT('Ctrl Pts',(64.8016959801978,4.78053723084404,9.63611017812334));
#4742=CARTESIAN_POINT('Ctrl Pts',(64.7397191574786,4.72423126735984,9.73245892539434));
#4743=CARTESIAN_POINT('Ctrl Pts',(64.6317941862906,4.66230376279031,9.88159348365645));
#4744=CARTESIAN_POINT('Ctrl Pts',(64.5841440169343,4.64359013296362,9.9429714500931));
#4745=CARTESIAN_POINT('Ctrl Pts',(64.5333054217746,4.63091018458433,10.0048610303352));
#4746=CARTESIAN_POINT('',(65.0333054217746,5.96601779663744,9.270879409431));
#4747=CARTESIAN_POINT('Origin',(65.0333054217745,7.97231715504529,8.48965548688909));
#4748=CARTESIAN_POINT('',(58.5152881956451,6.97352938622157,8.53887939213984));
#4749=CARTESIAN_POINT('',(58.5152881956451,8.08415833106712,7.49592939215974));
#4750=CARTESIAN_POINT('Ctrl Pts',(58.5152881956451,6.97352938622157,8.53887939213984));
#4751=CARTESIAN_POINT('Ctrl Pts',(58.4654152249681,6.97043778978238,8.47614871902753));
#4752=CARTESIAN_POINT('Ctrl Pts',(58.4186772780868,6.97325094564081,8.41245543210374));
#4753=CARTESIAN_POINT('Ctrl Pts',(58.3120945049187,6.99593092515002,8.25268283428458));
#4754=CARTESIAN_POINT('Ctrl Pts',(58.2507030237862,7.02653178775528,8.14503131472124));
#4755=CARTESIAN_POINT('Ctrl Pts',(58.1653214105115,7.12969016348498,7.93896896733498));
#4756=CARTESIAN_POINT('Ctrl Pts',(58.1417842183134,7.20268302921674,7.84058888958738));
#4757=CARTESIAN_POINT('Ctrl Pts',(58.1417842183134,7.37285706901645,7.68078482934798));
#4758=CARTESIAN_POINT('Ctrl Pts',(58.1653214105115,7.47562627611464,7.61411333455621));
#4759=CARTESIAN_POINT('Ctrl Pts',(58.2507030237862,7.68775937453466,7.52409728016453));
#4760=CARTESIAN_POINT('Ctrl Pts',(58.3120945049187,7.79711991247583,7.50031629621303));
#4761=CARTESIAN_POINT('Ctrl Pts',(58.4186772780868,7.95800132326607,7.48771327488625));
#4762=CARTESIAN_POINT('Ctrl Pts',(58.4654152249681,8.02174556555534,7.48890500472477));
#4763=CARTESIAN_POINT('Ctrl Pts',(58.5152881956451,8.08415833106712,7.49592939215974));
#4764=CARTESIAN_POINT('',(64.5333054217746,6.97352938622157,8.53887939213984));
#4765=CARTESIAN_POINT('',(65.0333054217745,6.97352938622157,8.53887939213985));
#4766=CARTESIAN_POINT('',(64.5333054217746,8.08415833106712,7.49592939215974));
#4767=CARTESIAN_POINT('Ctrl Pts',(64.5333054217746,8.08415833106712,7.49592939215974));
#4768=CARTESIAN_POINT('Ctrl Pts',(64.5841440169343,8.02137952295014,7.48886380762262));
#4769=CARTESIAN_POINT('Ctrl Pts',(64.6317941862906,7.95722277837072,7.48769469250372));
#4770=CARTESIAN_POINT('Ctrl Pts',(64.7397191574786,7.79625073359952,7.50050613631088));
#4771=CARTESIAN_POINT('Ctrl Pts',(64.8016959801978,7.68721813006929,7.52428288949533));
#4772=CARTESIAN_POINT('Ctrl Pts',(64.8879780992218,7.47551721277898,7.61420381102219));
#4773=CARTESIAN_POINT('Ctrl Pts',(64.9118211190309,7.37284953498186,7.68079190427738));
#4774=CARTESIAN_POINT('Ctrl Pts',(64.9118211190309,7.20269056325133,7.84058181465798));
#4775=CARTESIAN_POINT('Ctrl Pts',(64.8879780992218,7.12978730955983,7.93886580027521));
#4776=CARTESIAN_POINT('Ctrl Pts',(64.8016959801978,7.02675101584962,8.1445027927845));
#4777=CARTESIAN_POINT('Ctrl Pts',(64.7397191574786,6.99617496683501,8.25182729069262));
#4778=CARTESIAN_POINT('Ctrl Pts',(64.6317941862906,6.97328128516483,8.41167725669145));
#4779=CARTESIAN_POINT('Ctrl Pts',(64.5841440169343,6.97041965797865,8.47578081193636));
#4780=CARTESIAN_POINT('Ctrl Pts',(64.5333054217746,6.97352938622157,8.53887939213984));
#4781=CARTESIAN_POINT('',(65.0333054217745,8.08415833106713,7.49592939215974));
#4782=CARTESIAN_POINT('Origin',(65.0333054217745,9.83314361665672,6.24030269465341));
#4783=CARTESIAN_POINT('',(58.5152881956451,8.87797608967546,6.53636855793469));
#4784=CARTESIAN_POINT('',(58.5152881956451,9.69434146610128,5.2499825630792));
#4785=CARTESIAN_POINT('Ctrl Pts',(58.5152881956451,8.87797608967545,6.53636855793469));
#4786=CARTESIAN_POINT('Ctrl Pts',(58.4654152249681,8.85938113740538,6.47637753304147));
#4787=CARTESIAN_POINT('Ctrl Pts',(58.4186772780868,8.84626603646124,6.41398568443713));
#4788=CARTESIAN_POINT('Ctrl Pts',(58.3120945049187,8.82849965338492,6.25359235503467));
#4789=CARTESIAN_POINT('Ctrl Pts',(58.2507030237862,8.83136728936705,6.14171278084726));
#4790=CARTESIAN_POINT('Ctrl Pts',(58.1653214105115,8.88003913310781,5.91646981620596));
#4791=CARTESIAN_POINT('Ctrl Pts',(58.1417842183134,8.9262726633038,5.80302794196644));
#4792=CARTESIAN_POINT('Ctrl Pts',(58.1417842183134,9.0513587190056,5.6059238573824));
#4793=CARTESIAN_POINT('Ctrl Pts',(58.1653214105115,9.13431871596657,5.51578930768254));
#4794=CARTESIAN_POINT('Ctrl Pts',(58.2507030237862,9.31740118060456,5.37584591685752));
#4795=CARTESIAN_POINT('Ctrl Pts',(58.3120945049187,9.41741186593077,5.32561519640614));
#4796=CARTESIAN_POINT('Ctrl Pts',(58.4186772780868,9.57010464740912,5.27339854227333));
#4797=CARTESIAN_POINT('Ctrl Pts',(58.4654152249681,9.63214261826849,5.25870028330521));
#4798=CARTESIAN_POINT('Ctrl Pts',(58.5152881956451,9.69434146610128,5.24998256307919));
#4799=CARTESIAN_POINT('',(64.5333054217746,8.87797608967546,6.53636855793469));
#4800=CARTESIAN_POINT('',(65.0333054217745,8.87797608967545,6.5363685579347));
#4801=CARTESIAN_POINT('',(64.5333054217746,9.69434146610128,5.2499825630792));
#4802=CARTESIAN_POINT('Ctrl Pts',(64.5333054217746,9.69434146610128,5.24998256307919));
#4803=CARTESIAN_POINT('Ctrl Pts',(64.5841440169343,9.63177783026215,5.25875141157996));
#4804=CARTESIAN_POINT('Ctrl Pts',(64.6317941862906,9.5693459406827,5.2735741599327));
#4805=CARTESIAN_POINT('Ctrl Pts',(64.7397191574786,9.41661720521969,5.3260152283249));
#4806=CARTESIAN_POINT('Ctrl Pts',(64.8016959801978,9.31692309949288,5.37616029695489));
#4807=CARTESIAN_POINT('Ctrl Pts',(64.8879780992218,9.13423557963827,5.51590406461261));
#4808=CARTESIAN_POINT('Ctrl Pts',(64.9118211190309,9.05135318112996,5.60593258367809));
#4809=CARTESIAN_POINT('Ctrl Pts',(64.9118211190309,8.92627820117944,5.80301921567074));
#4810=CARTESIAN_POINT('Ctrl Pts',(64.8879780992218,8.88010757055562,5.91634573108269));
#4811=CARTESIAN_POINT('Ctrl Pts',(64.8016959801978,8.83144819194687,6.14114634358899));
#4812=CARTESIAN_POINT('Ctrl Pts',(64.7397191574786,8.82852326301226,6.25270299921878));
#4813=CARTESIAN_POINT('Ctrl Pts',(64.6317941862906,8.84610189845785,6.41322441170358));
#4814=CARTESIAN_POINT('Ctrl Pts',(64.5841440169343,8.8592720804726,6.47602569362431));
#4815=CARTESIAN_POINT('Ctrl Pts',(64.5333054217746,8.87797608967545,6.53636855793469));
#4816=CARTESIAN_POINT('',(65.0333054217745,9.69434146610128,5.24998256307919));
#4817=CARTESIAN_POINT('Origin',(65.0333054217745,11.0761175010611,3.59884873388474));
#4818=CARTESIAN_POINT('',(58.5152881956451,10.2245869045029,4.1231536481525));
#4819=CARTESIAN_POINT('',(58.5152881956451,10.6953934735264,2.67416002147514));
#4820=CARTESIAN_POINT('Ctrl Pts',(58.5152881956451,10.2245869045029,4.12315364815251));
#4821=CARTESIAN_POINT('Ctrl Pts',(58.4654152249681,10.1916569856405,4.06967172820395));
#4822=CARTESIAN_POINT('Ctrl Pts',(58.4186772780868,10.1634376979201,4.01250162722806));
#4823=CARTESIAN_POINT('Ctrl Pts',(58.3120945049187,10.1063412794472,3.86156566901406));
#4824=CARTESIAN_POINT('Ctrl Pts',(58.2507030237862,10.081295504691,3.75248784531307));
#4825=CARTESIAN_POINT('Ctrl Pts',(58.1653214105115,10.072422585498,3.52221710727082));
#4826=CARTESIAN_POINT('Ctrl Pts',(58.1417842183134,10.088991757421,3.40084140670787));
#4827=CARTESIAN_POINT('Ctrl Pts',(58.1417842183134,10.1611302121108,3.17882207231172));
#4828=CARTESIAN_POINT('Ctrl Pts',(58.1653214105115,10.21906831722,3.07088795295311));
#4829=CARTESIAN_POINT('Ctrl Pts',(58.2507030237862,10.3615964034925,2.88981038361606));
#4830=CARTESIAN_POINT('Ctrl Pts',(58.3120945049187,10.4459731970312,2.81628610756644));
#4831=CARTESIAN_POINT('Ctrl Pts',(58.4186772780868,10.5808831001726,2.72773678504619));
#4832=CARTESIAN_POINT('Ctrl Pts',(58.4654152249681,10.6373167257333,2.69807208293881));
#4833=CARTESIAN_POINT('Ctrl Pts',(58.5152881956451,10.6953934735264,2.67416002147513));
#4834=CARTESIAN_POINT('',(64.5333054217746,10.2245869045029,4.1231536481525));
#4835=CARTESIAN_POINT('',(65.0333054217745,10.2245869045029,4.12315364815251));
#4836=CARTESIAN_POINT('',(64.5333054217746,10.6953934735264,2.67416002147514));
#4837=CARTESIAN_POINT('Ctrl Pts',(64.5333054217746,10.6953934735264,2.67416002147513));
#4838=CARTESIAN_POINT('Ctrl Pts',(64.5841440169343,10.6369761132978,2.69821232401292));
#4839=CARTESIAN_POINT('Ctrl Pts',(64.6317941862906,10.580191903949,2.72809556804403));
#4840=CARTESIAN_POINT('Ctrl Pts',(64.7397191574786,10.4453029859404,2.81687119582944));
#4841=CARTESIAN_POINT('Ctrl Pts',(64.8016959801978,10.3612115253291,2.89023378082229));
#4842=CARTESIAN_POINT('Ctrl Pts',(64.8879780992218,10.2190163316603,3.07101977974729));
#4843=CARTESIAN_POINT('Ctrl Pts',(64.9118211190309,10.1611270183592,3.17883190166845));
#4844=CARTESIAN_POINT('Ctrl Pts',(64.9118211190309,10.0889949511726,3.40083157735114));
#4845=CARTESIAN_POINT('Ctrl Pts',(64.8879780992218,10.0724580141423,3.5220799008087));
#4846=CARTESIAN_POINT('Ctrl Pts',(64.8016959801978,10.0812329983496,3.75191908406943));
#4847=CARTESIAN_POINT('Ctrl Pts',(64.7397191574786,10.1061429735371,3.86069838247098));
#4848=CARTESIAN_POINT('Ctrl Pts',(64.6317941862906,10.1630893957837,4.01180509073886));
#4849=CARTESIAN_POINT('Ctrl Pts',(64.5841440169343,10.1914638560269,4.06935806382539));
#4850=CARTESIAN_POINT('Ctrl Pts',(64.5333054217746,10.2245869045029,4.1231536481525));
#4851=CARTESIAN_POINT('',(65.0333054217745,10.6953934735264,2.67416002147513));
#4852=CARTESIAN_POINT('Origin',(65.0333054217745,11.6231381877631,0.731265871526308));
#4853=CARTESIAN_POINT('',(58.5152881956451,10.9287493207203,1.45086583075851));
#4854=CARTESIAN_POINT('',(58.5152881956451,11.0244145741041,-0.0696898291507925));
#4855=CARTESIAN_POINT('Ctrl Pts',(58.5152881956451,10.9287493207203,1.45086583075852));
#4856=CARTESIAN_POINT('Ctrl Pts',(58.4654152249681,10.8835535431755,1.40725348147776));
#4857=CARTESIAN_POINT('Ctrl Pts',(58.4186772780868,10.8420031903095,1.35889733583154));
#4858=CARTESIAN_POINT('Ctrl Pts',(58.3120945049187,10.7491643143985,1.22690261016421));
#4859=CARTESIAN_POINT('Ctrl Pts',(58.2507030237862,10.6977788470438,1.12748029777294));
#4860=CARTESIAN_POINT('Ctrl Pts',(58.1653214105115,10.6319186830624,0.906650543677475));
#4861=CARTESIAN_POINT('Ctrl Pts',(58.1417842183134,10.6177823947033,0.784967498446075));
#4862=CARTESIAN_POINT('Ctrl Pts',(58.1417842183134,10.6324405239663,0.551983205547912));
#4863=CARTESIAN_POINT('Ctrl Pts',(58.1653214105115,10.6617162729982,0.433031414203771));
#4864=CARTESIAN_POINT('Ctrl Pts',(58.2507030237862,10.7547344170632,0.222197435992864));
#4865=CARTESIAN_POINT('Ctrl Pts',(58.3120945049187,10.8181756145601,0.129999405012576));
#4866=CARTESIAN_POINT('Ctrl Pts',(58.4186772780868,10.9268257539862,0.0106812937004497));
#4867=CARTESIAN_POINT('Ctrl Pts',(58.4654152249681,10.9741091020059,-0.0320859092136418));
#4868=CARTESIAN_POINT('Ctrl Pts',(58.5152881956451,11.0244145741041,-0.069689829150799));
#4869=CARTESIAN_POINT('',(64.5333054217746,10.9287493207203,1.45086583075851));
#4870=CARTESIAN_POINT('',(65.0333054217745,10.9287493207203,1.45086583075852));
#4871=CARTESIAN_POINT('',(64.5333054217746,11.0244145741041,-0.0696898291507925));
#4872=CARTESIAN_POINT('Ctrl Pts',(64.5333054217746,11.0244145741041,-0.0696898291507991));
#4873=CARTESIAN_POINT('Ctrl Pts',(64.5841440169343,10.9738140670733,-0.0318653672026165));
#4874=CARTESIAN_POINT('Ctrl Pts',(64.6317941862906,10.9262454986663,0.0112006983815072));
#4875=CARTESIAN_POINT('Ctrl Pts',(64.7397191574786,10.8176719649172,0.130732786372444));
#4876=CARTESIAN_POINT('Ctrl Pts',(64.8016959801978,10.7544669251584,0.222703246704341));
#4877=CARTESIAN_POINT('Ctrl Pts',(64.8879780992218,10.6616987046511,0.43317202769978));
#4878=CARTESIAN_POINT('Ctrl Pts',(64.9118211190309,10.6324398750139,0.551993520351058));
#4879=CARTESIAN_POINT('Ctrl Pts',(64.9118211190309,10.6177830436557,0.784957183642929));
#4880=CARTESIAN_POINT('Ctrl Pts',(64.8879780992218,10.6319188767911,0.906508837063128));
#4881=CARTESIAN_POINT('Ctrl Pts',(64.8016959801978,10.6975768592847,1.12694494990463));
#4882=CARTESIAN_POINT('Ctrl Pts',(64.7397191574786,10.7487565532408,1.22611188769709));
#4883=CARTESIAN_POINT('Ctrl Pts',(64.6317941862906,10.8414926091443,1.358309301536));
#4884=CARTESIAN_POINT('Ctrl Pts',(64.5841440169343,10.8832884759249,1.40699770082426));
#4885=CARTESIAN_POINT('Ctrl Pts',(64.5333054217746,10.9287493207203,1.45086583075852));
#4886=CARTESIAN_POINT('',(65.0333054217745,11.0244145741041,-0.0696898291508022));
#4887=CARTESIAN_POINT('Origin',(65.0333054217745,11.4398343552159,-2.18226511494788));
#4888=CARTESIAN_POINT('',(58.5152881956451,10.9462182239883,-1.31258522269331));
#4889=CARTESIAN_POINT('',(58.5152881956451,10.6607311620303,-2.80916081150993));
#4890=CARTESIAN_POINT('Ctrl Pts',(58.5152881956451,10.9462182239883,-1.3125852226933));
#4891=CARTESIAN_POINT('Ctrl Pts',(58.4654152249681,10.8915964046827,-1.34358767700596));
#4892=CARTESIAN_POINT('Ctrl Pts',(58.4186772780868,10.8393257481533,-1.38009147285009));
#4893=CARTESIAN_POINT('Ctrl Pts',(58.3120945049187,10.7165778228152,-1.48485125191443));
#4894=CARTESIAN_POINT('Ctrl Pts',(58.2507030237862,10.6420814007585,-1.56837098345874));
#4895=CARTESIAN_POINT('Ctrl Pts',(58.1653214105115,10.5233722283083,-1.76588420800259));
#4896=CARTESIAN_POINT('Ctrl Pts',(58.1417842183134,10.4794187146543,-1.88022880465161));
#4897=CARTESIAN_POINT('Ctrl Pts',(58.1417842183134,10.4356754943201,-2.1095387960727));
#4898=CARTESIAN_POINT('Ctrl Pts',(58.1653214105115,10.4344493842944,-2.23203408087814));
#4899=CARTESIAN_POINT('Ctrl Pts',(58.2507030237862,10.4721129140633,-2.45937699371878));
#4900=CARTESIAN_POINT('Ctrl Pts',(58.3120945049187,10.5106322717593,-2.56445563826261));
#4901=CARTESIAN_POINT('Ctrl Pts',(58.4186772780868,10.5861957596229,-2.70704534261155));
#4902=CARTESIAN_POINT('Ctrl Pts',(58.4654152249681,10.6213578434494,-2.76022782568649));
#4903=CARTESIAN_POINT('Ctrl Pts',(58.5152881956451,10.6607311620303,-2.80916081150993));
#4904=CARTESIAN_POINT('',(64.5333054217746,10.9462182239883,-1.31258522269331));
#4905=CARTESIAN_POINT('',(65.0333054217745,10.9462182239883,-1.3125852226933));
#4906=CARTESIAN_POINT('',(64.5333054217746,10.6607311620303,-2.80916081150993));
#4907=CARTESIAN_POINT('Ctrl Pts',(64.5333054217746,10.6607311620303,-2.80916081150993));
#4908=CARTESIAN_POINT('Ctrl Pts',(64.5841440169343,10.6211269241497,-2.75994084020421));
#4909=CARTESIAN_POINT('Ctrl Pts',(64.6317941862906,10.5857629047824,-2.70639795235363));
#4910=CARTESIAN_POINT('Ctrl Pts',(64.7397191574786,10.5103268297238,-2.5636200448539));
#4911=CARTESIAN_POINT('Ctrl Pts',(64.8016959801978,10.4719796159174,-2.4588205514493));
#4912=CARTESIAN_POINT('Ctrl Pts',(64.8879780992218,10.4344673370436,-2.2318935159434));
#4913=CARTESIAN_POINT('Ctrl Pts',(64.9118211190309,10.4356774309429,-2.10952864394017));
#4914=CARTESIAN_POINT('Ctrl Pts',(64.9118211190309,10.4794167780314,-1.88023895678415));
#4915=CARTESIAN_POINT('Ctrl Pts',(64.8879780992218,10.5233371749486,-1.76602151082142));
#4916=CARTESIAN_POINT('Ctrl Pts',(64.8016959801978,10.6417526232152,-1.5688392800763));
#4917=CARTESIAN_POINT('Ctrl Pts',(64.7397191574786,10.7159862275429,-1.4855157263049));
#4918=CARTESIAN_POINT('Ctrl Pts',(64.6317941862906,10.8386849696517,-1.38053405659455));
#4919=CARTESIAN_POINT('Ctrl Pts',(64.5841440169343,10.8912760549453,-1.34376950229525));
#4920=CARTESIAN_POINT('Ctrl Pts',(64.5333054217746,10.9462182239883,-1.3125852226933));
#4921=CARTESIAN_POINT('',(65.0333054217745,10.6607311620303,-2.80916081150994));
#4922=CARTESIAN_POINT('Origin',(65.0333054217745,10.5377236573627,-4.95867635844021));
#4923=CARTESIAN_POINT('',(58.5152881956451,10.2758959788686,-3.99356171925254));
#4924=CARTESIAN_POINT('',(58.5152881956451,9.62719480361945,-5.37212188871111));
#4925=CARTESIAN_POINT('Ctrl Pts',(58.5152881956451,10.2758959788686,-3.99356171925253));
#4926=CARTESIAN_POINT('Ctrl Pts',(58.4654152249681,10.2152802075941,-4.01000628037357));
#4927=CARTESIAN_POINT('Ctrl Pts',(58.4186772780868,10.155573604989,-4.03236405867114));
#4928=CARTESIAN_POINT('Ctrl Pts',(58.3120945049187,10.0106293338081,-4.10330644893436));
#4929=CARTESIAN_POINT('Ctrl Pts',(58.2507030237862,9.91770284122587,-4.16567574773471));
#4930=CARTESIAN_POINT('Ctrl Pts',(58.1653214105115,9.75360359419369,-4.32746196042601));
#4931=CARTESIAN_POINT('Ctrl Pts',(58.1417842183134,9.68259461615746,-4.4272834169552));
#4932=CARTESIAN_POINT('Ctrl Pts',(58.1417842183134,9.5831985936359,-4.63851071679507));
#4933=CARTESIAN_POINT('Ctrl Pts',(58.1653214105115,9.55154766555483,-4.75685266581133));
#4934=CARTESIAN_POINT('Ctrl Pts',(58.2507030237862,9.53149004293565,-4.98641972195918));
#4935=CARTESIAN_POINT('Ctrl Pts',(58.3120945049187,9.54266724792246,-5.09777650237764));
#4936=CARTESIAN_POINT('Ctrl Pts',(58.4186772780868,9.58039615237783,-5.2546783642309));
#4937=CARTESIAN_POINT('Ctrl Pts',(58.4654152249681,9.60122760896736,-5.3149344764636));
#4938=CARTESIAN_POINT('Ctrl Pts',(58.5152881956451,9.62719480361944,-5.37212188871111));
#4939=CARTESIAN_POINT('',(64.5333054217746,10.2758959788686,-3.99356171925254));
#4940=CARTESIAN_POINT('',(65.0333054217745,10.2758959788686,-3.99356171925253));
#4941=CARTESIAN_POINT('',(64.5333054217746,9.62719480361945,-5.37212188871111));
#4942=CARTESIAN_POINT('Ctrl Pts',(64.5333054217746,9.62719480361944,-5.37212188871111));
#4943=CARTESIAN_POINT('Ctrl Pts',(64.5841440169343,9.60107531480922,-5.31459907986337));
#4944=CARTESIAN_POINT('Ctrl Pts',(64.6317941862906,9.58013789587829,-5.25394366630695));
#4945=CARTESIAN_POINT('Ctrl Pts',(64.7397191574786,9.54257920554065,-5.09689120032706));
#4946=CARTESIAN_POINT('Ctrl Pts',(64.8016959801978,9.53149931416127,-4.98584761144596));
#4947=CARTESIAN_POINT('Ctrl Pts',(64.8879780992218,9.55160001136319,-4.75672098164969));
#4948=CARTESIAN_POINT('Ctrl Pts',(64.9118211190309,9.58320299414889,-4.63850136522897));
#4949=CARTESIAN_POINT('Ctrl Pts',(64.9118211190309,9.68259021564447,-4.42729276852131));
#4950=CARTESIAN_POINT('Ctrl Pts',(64.8879780992218,9.75353549627729,-4.32758623220826));
#4951=CARTESIAN_POINT('Ctrl Pts',(64.8016959801978,9.91726793220073,-4.16604756830275));
#4952=CARTESIAN_POINT('Ctrl Pts',(64.7397191574786,10.009891076528,-4.10380292387847));
#4953=CARTESIAN_POINT('Ctrl Pts',(64.6317941862906,10.1548428916209,-4.03263338270016));
#4954=CARTESIAN_POINT('Ctrl Pts',(64.5841440169343,10.2149247041221,-4.010102725547));
#4955=CARTESIAN_POINT('Ctrl Pts',(64.5333054217746,10.2758959788686,-3.99356171925253));
#4956=CARTESIAN_POINT('',(65.0333054217745,9.62719480361944,-5.37212188871111));
#4957=CARTESIAN_POINT('Origin',(65.0333054217745,8.9734890270808,-7.42351572959578));
#4958=CARTESIAN_POINT('',(58.5152881956451,8.9599013972947,-6.42360804569852));
#4959=CARTESIAN_POINT('',(58.5152881956451,7.98874638935144,-7.59753279036232));
#4960=CARTESIAN_POINT('Ctrl Pts',(58.5152881956451,8.9599013972947,-6.42360804569851));
#4961=CARTESIAN_POINT('Ctrl Pts',(58.4654152249681,8.89710038588973,-6.42446144137384));
#4962=CARTESIAN_POINT('Ctrl Pts',(58.4186772780868,8.83370942263619,-6.43126838068827));
#4963=CARTESIAN_POINT('Ctrl Pts',(58.3120945049187,8.67567618723855,-6.46393581086227));
#4964=CARTESIAN_POINT('Ctrl Pts',(58.2507030237862,8.57015853741945,-6.50123578449678));
#4965=CARTESIAN_POINT('Ctrl Pts',(58.1653214105115,8.37098017501116,-6.61712936258408));
#4966=CARTESIAN_POINT('Ctrl Pts',(58.1417842183134,8.27737748783543,-6.69615552976207));
#4967=CARTESIAN_POINT('Ctrl Pts',(58.1417842183134,8.12857408077458,-6.87602794993212));
#4968=CARTESIAN_POINT('Ctrl Pts',(58.1653214105115,8.06848707885344,-6.98278070327126));
#4969=CARTESIAN_POINT('Ctrl Pts',(58.2507030237862,7.99196859804205,-7.20014736029998));
#4970=CARTESIAN_POINT('Ctrl Pts',(58.3120945049187,7.97510134542345,-7.31078532053779));
#4971=CARTESIAN_POINT('Ctrl Pts',(58.4186772780868,7.9726250206465,-7.47214061887044));
#4972=CARTESIAN_POINT('Ctrl Pts',(58.4654152249681,7.97781693296876,-7.53568424712284));
#4973=CARTESIAN_POINT('Ctrl Pts',(58.5152881956451,7.98874638935144,-7.59753279036232));
#4974=CARTESIAN_POINT('',(64.5333054217746,8.9599013972947,-6.42360804569852));
#4975=CARTESIAN_POINT('',(65.0333054217745,8.95990139729471,-6.42360804569851));
#4976=CARTESIAN_POINT('',(64.5333054217746,7.98874638935144,-7.59753279036232));
#4977=CARTESIAN_POINT('Ctrl Pts',(64.5333054217746,7.98874638935144,-7.59753279036232));
#4978=CARTESIAN_POINT('Ctrl Pts',(64.5841440169343,7.97775283315432,-7.53532151360656));
#4979=CARTESIAN_POINT('Ctrl Pts',(64.6317941862906,7.97255758969361,-7.47136477705306));
#4980=CARTESIAN_POINT('Ctrl Pts',(64.7397191574786,7.97523623472203,-7.30990593662908));
#4981=CARTESIAN_POINT('Ctrl Pts',(64.8016959801978,7.99211985609405,-7.19959552935062));
#4982=CARTESIAN_POINT('Ctrl Pts',(64.8879780992218,8.06857052864127,-6.98266617408288));
#4983=CARTESIAN_POINT('Ctrl Pts',(64.9118211190309,8.12858066867727,-6.87601998652573));
#4984=CARTESIAN_POINT('Ctrl Pts',(64.9118211190309,8.27737089993274,-6.69616349316845));
#4985=CARTESIAN_POINT('Ctrl Pts',(64.8879780992218,8.37088331138052,-6.61723279487663));
#4986=CARTESIAN_POINT('Ctrl Pts',(64.8016959801978,8.56964482384595,-6.50148776616156));
#4987=CARTESIAN_POINT('Ctrl Pts',(64.7397191574786,8.67483765537062,-6.46423309101336));
#4988=CARTESIAN_POINT('Ctrl Pts',(64.6317941862906,8.8329346878098,-6.43134752238259));
#4989=CARTESIAN_POINT('Ctrl Pts',(64.5841440169343,8.89673206627378,-6.42446644642647));
#4990=CARTESIAN_POINT('Ctrl Pts',(64.5333054217746,8.9599013972947,-6.42360804569851));
#4991=CARTESIAN_POINT('',(65.0333054217745,7.98874638935144,-7.59753279036232));
#4992=CARTESIAN_POINT('Origin',(65.0333054217745,6.8454170790433,-9.42190830567978));
#4993=CARTESIAN_POINT('',(58.5152881956451,7.08092325871652,-8.45003545425543));
#4994=CARTESIAN_POINT('',(58.5152881956451,5.84833565888647,-9.34556276502401));
#4995=CARTESIAN_POINT('Ctrl Pts',(58.5152881956451,7.08092325871652,-8.45003545425542));
#4996=CARTESIAN_POINT('Ctrl Pts',(58.4654152249681,7.01988302569362,-8.43524406249618));
#4997=CARTESIAN_POINT('Ctrl Pts',(58.4186772780868,6.95679078914847,-8.42607245779616));
#4998=CARTESIAN_POINT('Ctrl Pts',(58.3120945049187,6.79559839891971,-8.41841231310071));
#4999=CARTESIAN_POINT('Ctrl Pts',(58.2507030237862,6.68411965386863,-8.42829926704623));
#5000=CARTESIAN_POINT('Ctrl Pts',(58.1653214105115,6.46237728512112,-8.49101819079154));
#5001=CARTESIAN_POINT('Ctrl Pts',(58.1417842183134,6.35206228988776,-8.54428356389661));
#5002=CARTESIAN_POINT('Ctrl Pts',(58.1417842183134,6.16320136361389,-8.68149905871306));
#5003=CARTESIAN_POINT('Ctrl Pts',(58.1653214105115,6.07845377516792,-8.76995494827363));
#5004=CARTESIAN_POINT('Ctrl Pts',(58.2507030237862,5.95028237372899,-8.96146325970346));
#5005=CARTESIAN_POINT('Ctrl Pts',(58.3120945049187,5.90643049502042,-9.06443060982093));
#5006=CARTESIAN_POINT('Ctrl Pts',(58.4186772780868,5.86390453760418,-9.22010079781545));
#5007=CARTESIAN_POINT('Ctrl Pts',(58.4654152249681,5.85313067871345,-9.28293926222734));
#5008=CARTESIAN_POINT('Ctrl Pts',(58.5152881956451,5.84833565888646,-9.34556276502401));
#5009=CARTESIAN_POINT('',(64.5333054217746,7.08092325871652,-8.45003545425543));
#5010=CARTESIAN_POINT('',(65.0333054217745,7.08092325871653,-8.45003545425542));
#5011=CARTESIAN_POINT('',(64.5333054217746,5.84833565888647,-9.34556276502401));
#5012=CARTESIAN_POINT('Ctrl Pts',(64.5333054217746,5.84833565888646,-9.34556276502401));
#5013=CARTESIAN_POINT('Ctrl Pts',(64.5841440169343,5.85315880086979,-9.28257198367587));
#5014=CARTESIAN_POINT('Ctrl Pts',(64.6317941862906,5.86403216913269,-9.21933256109938));
#5015=CARTESIAN_POINT('Ctrl Pts',(64.7397191574786,5.90677984040867,-9.06361239897923));
#5016=CARTESIAN_POINT('Ctrl Pts',(64.8016959801978,5.95056611450767,-8.96096638188601));
#5017=CARTESIAN_POINT('Ctrl Pts',(64.8879780992218,6.07856308547815,-8.76986477034863));
#5018=CARTESIAN_POINT('Ctrl Pts',(64.9118211190309,6.16320972496414,-8.68149298383651));
#5019=CARTESIAN_POINT('Ctrl Pts',(64.9118211190309,6.35205392853751,-8.54428963877316));
#5020=CARTESIAN_POINT('Ctrl Pts',(64.8879780992218,6.4622577420744,-8.49109428456304));
#5021=CARTESIAN_POINT('Ctrl Pts',(64.8016959801978,6.68355941425992,-8.42841557687301));
#5022=CARTESIAN_POINT('Ctrl Pts',(64.7397191574786,6.79471228050513,-8.41849171925358));
#5023=CARTESIAN_POINT('Ctrl Pts',(64.6317941862906,6.95602071230226,-8.42595644439207));
#5024=CARTESIAN_POINT('Ctrl Pts',(64.5841440169343,7.01952503280972,-8.43515731294215));
#5025=CARTESIAN_POINT('Ctrl Pts',(64.5333054217746,7.08092325871652,-8.45003545425542));
#5026=CARTESIAN_POINT('',(65.0333054217745,5.84833565888646,-9.34556276502402));
#5027=CARTESIAN_POINT('Origin',(65.0333054217745,4.28722240024657,-10.8282877315631));
#5028=CARTESIAN_POINT('',(58.5152881956451,4.75702466997909,-9.94551605816494));
#5029=CARTESIAN_POINT('',(58.5152881956451,3.34045249029966,-10.5063766605837));
#5030=CARTESIAN_POINT('Ctrl Pts',(58.5152881956451,4.7570246699791,-9.94551605816493));
#5031=CARTESIAN_POINT('Ctrl Pts',(58.4654152249681,4.70158059766936,-9.91600927651429));
#5032=CARTESIAN_POINT('Ctrl Pts',(58.4186772780868,4.64275140509176,-9.89143541345394));
#5033=CARTESIAN_POINT('Ctrl Pts',(58.3120945049187,4.48852817073407,-9.84392900895229));
#5034=CARTESIAN_POINT('Ctrl Pts',(58.2507030237862,4.37809294999274,-9.82578170953074));
#5035=CARTESIAN_POINT('Ctrl Pts',(58.1653214105115,4.1477194634458,-9.83138511829107));
#5036=CARTESIAN_POINT('Ctrl Pts',(58.1417842183134,4.02762365701549,-9.8555428380347));
#5037=CARTESIAN_POINT('Ctrl Pts',(58.1417842183134,3.81057203810829,-9.94147965331495));
#5038=CARTESIAN_POINT('Ctrl Pts',(58.1653214105115,3.70648886579938,-10.0060806702378));
#5039=CARTESIAN_POINT('Ctrl Pts',(58.2507030237862,3.53471802426675,-10.1596974645434));
#5040=CARTESIAN_POINT('Ctrl Pts',(58.3120945049187,3.46663689428341,-10.2485243872452));
#5041=CARTESIAN_POINT('Ctrl Pts',(58.4186772780868,3.38673336653187,-10.388728134475));
#5042=CARTESIAN_POINT('Ctrl Pts',(58.4654152249681,3.36067069760572,-10.4469130632236));
#5043=CARTESIAN_POINT('Ctrl Pts',(58.5152881956451,3.34045249029966,-10.5063766605837));
#5044=CARTESIAN_POINT('',(64.5333054217746,4.75702466997909,-9.94551605816494));
#5045=CARTESIAN_POINT('',(65.0333054217745,4.7570246699791,-9.94551605816493));
#5046=CARTESIAN_POINT('',(64.5333054217746,3.34045249029966,-10.5063766605837));
#5047=CARTESIAN_POINT('Ctrl Pts',(64.5333054217746,3.34045249029966,-10.5063766605837));
#5048=CARTESIAN_POINT('Ctrl Pts',(64.5841440169343,3.36078927471434,-10.4465643170991));
#5049=CARTESIAN_POINT('Ctrl Pts',(64.6317941862906,3.38704804098346,-10.3880157739984));
#5050=CARTESIAN_POINT('Ctrl Pts',(64.7397191574787,3.46717874510578,-10.2478187606668));
#5051=CARTESIAN_POINT('Ctrl Pts',(64.8016959801978,3.53511641929548,-10.1592867605185));
#5052=CARTESIAN_POINT('Ctrl Pts',(64.8879780992218,3.7066171682632,-10.0060205097869));
#5053=CARTESIAN_POINT('Ctrl Pts',(64.911821119031,3.81058164753171,-9.94147584867507));
#5054=CARTESIAN_POINT('Ctrl Pts',(64.911821119031,4.02761404759207,-9.85554664267458));
#5055=CARTESIAN_POINT('Ctrl Pts',(64.8879780992218,4.14758475231227,-9.83142909229001));
#5056=CARTESIAN_POINT('Ctrl Pts',(64.8016959801978,4.37752138626385,-9.82575503934536));
#5057=CARTESIAN_POINT('Ctrl Pts',(64.7397191574786,4.48765014385175,-9.84378555172631));
#5058=CARTESIAN_POINT('Ctrl Pts',(64.6317941862906,4.64203437298612,-9.89113153450027));
#5059=CARTESIAN_POINT('Ctrl Pts',(64.5841440169343,4.70125542552701,-9.91583622314711));
#5060=CARTESIAN_POINT('Ctrl Pts',(64.5333054217746,4.7570246699791,-9.94551605816493));
#5061=CARTESIAN_POINT('',(65.0333054217745,3.34045249029966,-10.5063766605837));
#5062=CARTESIAN_POINT('Origin',(65.0333054217745,1.45964577074129,-11.5542860156157));
#5063=CARTESIAN_POINT('',(58.5152881956451,2.13422472611394,-10.8160833110905));
#5064=CARTESIAN_POINT('',(58.5152881956451,0.622676406422437,-11.0070362708084));
#5065=CARTESIAN_POINT('Ctrl Pts',(58.5152881956451,2.13422472611394,-10.8160833110905));
#5066=CARTESIAN_POINT('Ctrl Pts',(58.4654152249681,2.08786056948963,-10.7737151591579));
#5067=CARTESIAN_POINT('Ctrl Pts',(58.4186772780868,2.03699087540786,-10.7352831039296));
#5068=CARTESIAN_POINT('Ctrl Pts',(58.3120945049187,1.89942720992933,-10.650915441733));
#5069=CARTESIAN_POINT('Ctrl Pts',(58.2507030237862,1.79697456456924,-10.6058741505081));
#5070=CARTESIAN_POINT('Ctrl Pts',(58.1653214105115,1.57244517363704,-10.5540099615032));
#5071=CARTESIAN_POINT('Ctrl Pts',(58.1417842183134,1.45011461720928,-10.547542109508));
#5072=CARTESIAN_POINT('Ctrl Pts',(58.1417842183134,1.2185104571447,-10.5768005190945));
#5073=CARTESIAN_POINT('Ctrl Pts',(58.1653214105115,1.10163162948015,-10.6134875439005));
#5074=CARTESIAN_POINT('Ctrl Pts',(58.2507030237862,0.897054341556291,-10.7195605129324));
#5075=CARTESIAN_POINT('Ctrl Pts',(58.3120945049187,0.809021748079895,-10.7886656859827));
#5076=CARTESIAN_POINT('Ctrl Pts',(58.4186772780868,0.696761282506315,-10.904593475376));
#5077=CARTESIAN_POINT('Ctrl Pts',(58.4654152249681,0.657047416885181,-10.9544688953989));
#5078=CARTESIAN_POINT('Ctrl Pts',(58.5152881956451,0.622676406422432,-11.0070362708084));
#5079=CARTESIAN_POINT('',(64.5333054217746,2.13422472611394,-10.8160833110905));
#5080=CARTESIAN_POINT('',(65.0333054217745,2.13422472611395,-10.8160833110905));
#5081=CARTESIAN_POINT('',(64.5333054217746,0.622676406422437,-11.0070362708084));
#5082=CARTESIAN_POINT('Ctrl Pts',(64.5333054217746,0.622676406422433,-11.0070362708084));
#5083=CARTESIAN_POINT('Ctrl Pts',(64.5841440169343,0.657248998310229,-10.954160594703));
#5084=CARTESIAN_POINT('Ctrl Pts',(64.6317941862906,0.697243227727885,-10.9039817513676));
#5085=CARTESIAN_POINT('Ctrl Pts',(64.7397191574786,0.809722057856438,-10.7881169807807));
#5086=CARTESIAN_POINT('Ctrl Pts',(64.8016959801978,0.897542358210194,-10.7192617887444));
#5087=CARTESIAN_POINT('Ctrl Pts',(64.8879780992218,1.10177086238189,-10.613461181026));
#5088=CARTESIAN_POINT('Ctrl Pts',(64.9118211190309,1.21852071084588,-10.5767992237508));
#5089=CARTESIAN_POINT('Ctrl Pts',(64.9118211190309,1.4501043635081,-10.5475434048517));
#5090=CARTESIAN_POINT('Ctrl Pts',(64.8879780992218,1.57230375881265,-10.5540190526815));
#5091=CARTESIAN_POINT('Ctrl Pts',(64.8016959801978,1.79642759017132,-10.6057061760964));
#5092=CARTESIAN_POINT('Ctrl Pts',(64.7397191574786,1.89861244423744,-10.6505581350733));
#5093=CARTESIAN_POINT('Ctrl Pts',(64.6317941862906,2.03637194180704,-10.7348104532587));
#5094=CARTESIAN_POINT('Ctrl Pts',(64.5841440169343,2.08758864985044,-10.7734666755571));
#5095=CARTESIAN_POINT('Ctrl Pts',(64.5333054217746,2.13422472611394,-10.8160833110905));
#5096=CARTESIAN_POINT('',(65.0333054217745,0.622676406422429,-11.0070362708084));
#5097=CARTESIAN_POINT('Origin',(65.0333054217745,-1.45964577074129,-11.5542860156157));
#5098=CARTESIAN_POINT('',(58.5152881956451,-0.622676406422435,-11.0070362708084));
#5099=CARTESIAN_POINT('',(58.5152881956451,-2.13422472611394,-10.8160833110905));
#5100=CARTESIAN_POINT('Ctrl Pts',(58.5152881956451,-0.62267640642243,-11.0070362708084));
#5101=CARTESIAN_POINT('Ctrl Pts',(58.4654152249681,-0.657047416885175,-10.9544688953989));
#5102=CARTESIAN_POINT('Ctrl Pts',(58.4186772780868,-0.696761282506316,-10.904593475376));
#5103=CARTESIAN_POINT('Ctrl Pts',(58.3120945049187,-0.809021748079893,-10.7886656859827));
#5104=CARTESIAN_POINT('Ctrl Pts',(58.2507030237862,-0.897054341556289,-10.7195605129324));
#5105=CARTESIAN_POINT('Ctrl Pts',(58.1653214105115,-1.10163162948015,-10.6134875439005));
#5106=CARTESIAN_POINT('Ctrl Pts',(58.1417842183134,-1.2185104571447,-10.5768005190945));
#5107=CARTESIAN_POINT('Ctrl Pts',(58.1417842183134,-1.45011461720927,-10.547542109508));
#5108=CARTESIAN_POINT('Ctrl Pts',(58.1653214105115,-1.57244517363704,-10.5540099615032));
#5109=CARTESIAN_POINT('Ctrl Pts',(58.2507030237862,-1.79697456456924,-10.6058741505081));
#5110=CARTESIAN_POINT('Ctrl Pts',(58.3120945049187,-1.89942720992933,-10.650915441733));
#5111=CARTESIAN_POINT('Ctrl Pts',(58.4186772780868,-2.03699087540785,-10.7352831039296));
#5112=CARTESIAN_POINT('Ctrl Pts',(58.4654152249681,-2.08786056948963,-10.7737151591579));
#5113=CARTESIAN_POINT('Ctrl Pts',(58.5152881956451,-2.13422472611394,-10.8160833110905));
#5114=CARTESIAN_POINT('',(64.5333054217746,-0.622676406422435,-11.0070362708084));
#5115=CARTESIAN_POINT('',(65.0333054217745,-0.622676406422428,-11.0070362708084));
#5116=CARTESIAN_POINT('',(64.5333054217746,-2.13422472611394,-10.8160833110905));
#5117=CARTESIAN_POINT('Ctrl Pts',(64.5333054217746,-2.13422472611394,-10.8160833110905));
#5118=CARTESIAN_POINT('Ctrl Pts',(64.5841440169343,-2.08758864985044,-10.7734666755571));
#5119=CARTESIAN_POINT('Ctrl Pts',(64.6317941862906,-2.03637194180704,-10.7348104532587));
#5120=CARTESIAN_POINT('Ctrl Pts',(64.7397191574786,-1.89861244423744,-10.6505581350733));
#5121=CARTESIAN_POINT('Ctrl Pts',(64.8016959801978,-1.79642759017132,-10.6057061760964));
#5122=CARTESIAN_POINT('Ctrl Pts',(64.8879780992218,-1.57230375881265,-10.5540190526815));
#5123=CARTESIAN_POINT('Ctrl Pts',(64.9118211190309,-1.45010436350809,-10.5475434048517));
#5124=CARTESIAN_POINT('Ctrl Pts',(64.9118211190309,-1.21852071084588,-10.5767992237508));
#5125=CARTESIAN_POINT('Ctrl Pts',(64.8879780992218,-1.10177086238189,-10.613461181026));
#5126=CARTESIAN_POINT('Ctrl Pts',(64.8016959801978,-0.897542358210193,-10.7192617887444));
#5127=CARTESIAN_POINT('Ctrl Pts',(64.7397191574786,-0.809722057856437,-10.7881169807807));
#5128=CARTESIAN_POINT('Ctrl Pts',(64.6317941862906,-0.697243227727883,-10.9039817513676));
#5129=CARTESIAN_POINT('Ctrl Pts',(64.5841440169343,-0.657248998310227,-10.954160594703));
#5130=CARTESIAN_POINT('Ctrl Pts',(64.5333054217746,-0.622676406422431,-11.0070362708084));
#5131=CARTESIAN_POINT('',(65.0333054217745,-2.13422472611394,-10.8160833110905));
#5132=CARTESIAN_POINT('Origin',(65.0333054217745,-4.28722240024656,-10.8282877315631));
#5133=CARTESIAN_POINT('',(58.5152881956451,-3.34045249029966,-10.5063766605837));
#5134=CARTESIAN_POINT('',(58.5152881956451,-4.75702466997909,-9.94551605816494));
#5135=CARTESIAN_POINT('Ctrl Pts',(58.5152881956451,-3.34045249029965,-10.5063766605837));
#5136=CARTESIAN_POINT('Ctrl Pts',(58.4654152249681,-3.36067069760572,-10.4469130632236));
#5137=CARTESIAN_POINT('Ctrl Pts',(58.4186772780868,-3.38673336653187,-10.388728134475));
#5138=CARTESIAN_POINT('Ctrl Pts',(58.3120945049187,-3.4666368942834,-10.2485243872452));
#5139=CARTESIAN_POINT('Ctrl Pts',(58.2507030237862,-3.53471802426675,-10.1596974645434));
#5140=CARTESIAN_POINT('Ctrl Pts',(58.1653214105115,-3.70648886579937,-10.0060806702378));
#5141=CARTESIAN_POINT('Ctrl Pts',(58.1417842183134,-3.81057203810828,-9.94147965331495));
#5142=CARTESIAN_POINT('Ctrl Pts',(58.1417842183134,-4.02762365701548,-9.8555428380347));
#5143=CARTESIAN_POINT('Ctrl Pts',(58.1653214105115,-4.1477194634458,-9.83138511829107));
#5144=CARTESIAN_POINT('Ctrl Pts',(58.2507030237862,-4.37809294999273,-9.82578170953074));
#5145=CARTESIAN_POINT('Ctrl Pts',(58.3120945049187,-4.48852817073407,-9.84392900895229));
#5146=CARTESIAN_POINT('Ctrl Pts',(58.4186772780868,-4.64275140509175,-9.89143541345394));
#5147=CARTESIAN_POINT('Ctrl Pts',(58.4654152249681,-4.70158059766935,-9.91600927651429));
#5148=CARTESIAN_POINT('Ctrl Pts',(58.5152881956451,-4.75702466997909,-9.94551605816493));
#5149=CARTESIAN_POINT('',(64.5333054217746,-3.34045249029966,-10.5063766605837));
#5150=CARTESIAN_POINT('',(65.0333054217745,-3.34045249029965,-10.5063766605837));
#5151=CARTESIAN_POINT('',(64.5333054217746,-4.75702466997909,-9.94551605816494));
#5152=CARTESIAN_POINT('Ctrl Pts',(64.5333054217746,-4.75702466997909,-9.94551605816493));
#5153=CARTESIAN_POINT('Ctrl Pts',(64.5841440169343,-4.70125542552701,-9.91583622314712));
#5154=CARTESIAN_POINT('Ctrl Pts',(64.6317941862906,-4.64203437298611,-9.89113153450027));
#5155=CARTESIAN_POINT('Ctrl Pts',(64.7397191574786,-4.48765014385175,-9.84378555172631));
#5156=CARTESIAN_POINT('Ctrl Pts',(64.8016959801978,-4.37752138626384,-9.82575503934536));
#5157=CARTESIAN_POINT('Ctrl Pts',(64.8879780992218,-4.14758475231227,-9.83142909229001));
#5158=CARTESIAN_POINT('Ctrl Pts',(64.911821119031,-4.02761404759206,-9.85554664267458));
#5159=CARTESIAN_POINT('Ctrl Pts',(64.911821119031,-3.81058164753171,-9.94147584867507));
#5160=CARTESIAN_POINT('Ctrl Pts',(64.8879780992218,-3.70661716826319,-10.0060205097869));
#5161=CARTESIAN_POINT('Ctrl Pts',(64.8016959801978,-3.53511641929547,-10.1592867605185));
#5162=CARTESIAN_POINT('Ctrl Pts',(64.7397191574786,-3.46717874510578,-10.2478187606668));
#5163=CARTESIAN_POINT('Ctrl Pts',(64.6317941862906,-3.38704804098345,-10.3880157739984));
#5164=CARTESIAN_POINT('Ctrl Pts',(64.5841440169343,-3.36078927471433,-10.4465643170991));
#5165=CARTESIAN_POINT('Ctrl Pts',(64.5333054217746,-3.34045249029965,-10.5063766605837));
#5166=CARTESIAN_POINT('',(65.0333054217745,-4.7570246699791,-9.94551605816494));
#5167=CARTESIAN_POINT('Origin',(65.0333054217745,-6.8454170790433,-9.42190830567978));
#5168=CARTESIAN_POINT('',(58.5152881956451,-5.84833565888647,-9.34556276502401));
#5169=CARTESIAN_POINT('',(58.5152881956451,-7.08092325871652,-8.45003545425543));
#5170=CARTESIAN_POINT('Ctrl Pts',(58.5152881956451,-5.84833565888646,-9.34556276502402));
#5171=CARTESIAN_POINT('Ctrl Pts',(58.4654152249681,-5.85313067871344,-9.28293926222734));
#5172=CARTESIAN_POINT('Ctrl Pts',(58.4186772780868,-5.86390453760418,-9.22010079781545));
#5173=CARTESIAN_POINT('Ctrl Pts',(58.3120945049187,-5.90643049502042,-9.06443060982092));
#5174=CARTESIAN_POINT('Ctrl Pts',(58.2507030237862,-5.95028237372899,-8.96146325970346));
#5175=CARTESIAN_POINT('Ctrl Pts',(58.1653214105115,-6.07845377516792,-8.76995494827363));
#5176=CARTESIAN_POINT('Ctrl Pts',(58.1417842183134,-6.16320136361389,-8.68149905871306));
#5177=CARTESIAN_POINT('Ctrl Pts',(58.1417842183134,-6.35206228988776,-8.54428356389661));
#5178=CARTESIAN_POINT('Ctrl Pts',(58.1653214105115,-6.46237728512112,-8.49101819079154));
#5179=CARTESIAN_POINT('Ctrl Pts',(58.2507030237862,-6.68411965386863,-8.42829926704623));
#5180=CARTESIAN_POINT('Ctrl Pts',(58.3120945049187,-6.7955983989197,-8.41841231310071));
#5181=CARTESIAN_POINT('Ctrl Pts',(58.4186772780868,-6.95679078914847,-8.42607245779616));
#5182=CARTESIAN_POINT('Ctrl Pts',(58.4654152249681,-7.01988302569362,-8.43524406249618));
#5183=CARTESIAN_POINT('Ctrl Pts',(58.5152881956451,-7.08092325871652,-8.45003545425542));
#5184=CARTESIAN_POINT('',(64.5333054217746,-5.84833565888647,-9.34556276502401));
#5185=CARTESIAN_POINT('',(65.0333054217745,-5.84833565888646,-9.34556276502402));
#5186=CARTESIAN_POINT('',(64.5333054217746,-7.08092325871652,-8.45003545425543));
#5187=CARTESIAN_POINT('Ctrl Pts',(64.5333054217746,-7.08092325871652,-8.45003545425542));
#5188=CARTESIAN_POINT('Ctrl Pts',(64.5841440169343,-7.01952503280971,-8.43515731294215));
#5189=CARTESIAN_POINT('Ctrl Pts',(64.6317941862906,-6.95602071230226,-8.42595644439207));
#5190=CARTESIAN_POINT('Ctrl Pts',(64.7397191574786,-6.79471228050513,-8.41849171925358));
#5191=CARTESIAN_POINT('Ctrl Pts',(64.8016959801978,-6.68355941425992,-8.42841557687302));
#5192=CARTESIAN_POINT('Ctrl Pts',(64.8879780992218,-6.4622577420744,-8.49109428456304));
#5193=CARTESIAN_POINT('Ctrl Pts',(64.911821119031,-6.35205392853751,-8.54428963877316));
#5194=CARTESIAN_POINT('Ctrl Pts',(64.911821119031,-6.16320972496414,-8.68149298383651));
#5195=CARTESIAN_POINT('Ctrl Pts',(64.8879780992218,-6.07856308547815,-8.76986477034863));
#5196=CARTESIAN_POINT('Ctrl Pts',(64.8016959801978,-5.95056611450767,-8.96096638188601));
#5197=CARTESIAN_POINT('Ctrl Pts',(64.7397191574786,-5.90677984040867,-9.06361239897923));
#5198=CARTESIAN_POINT('Ctrl Pts',(64.6317941862906,-5.86403216913269,-9.21933256109938));
#5199=CARTESIAN_POINT('Ctrl Pts',(64.5841440169343,-5.85315880086979,-9.28257198367587));
#5200=CARTESIAN_POINT('Ctrl Pts',(64.5333054217746,-5.84833565888646,-9.34556276502402));
#5201=CARTESIAN_POINT('',(65.0333054217745,-7.08092325871653,-8.45003545425542));
#5202=CARTESIAN_POINT('Origin',(65.0333054217745,-8.97348902708079,-7.42351572959578));
#5203=CARTESIAN_POINT('',(58.5152881956451,-7.98874638935144,-7.59753279036232));
#5204=CARTESIAN_POINT('',(58.5152881956451,-8.9599013972947,-6.42360804569852));
#5205=CARTESIAN_POINT('Ctrl Pts',(58.5152881956451,-7.98874638935143,-7.59753279036232));
#5206=CARTESIAN_POINT('Ctrl Pts',(58.4654152249681,-7.97781693296876,-7.53568424712285));
#5207=CARTESIAN_POINT('Ctrl Pts',(58.4186772780868,-7.9726250206465,-7.47214061887045));
#5208=CARTESIAN_POINT('Ctrl Pts',(58.3120945049187,-7.97510134542344,-7.31078532053779));
#5209=CARTESIAN_POINT('Ctrl Pts',(58.2507030237862,-7.99196859804204,-7.20014736029998));
#5210=CARTESIAN_POINT('Ctrl Pts',(58.1653214105115,-8.06848707885343,-6.98278070327126));
#5211=CARTESIAN_POINT('Ctrl Pts',(58.1417842183134,-8.12857408077458,-6.87602794993212));
#5212=CARTESIAN_POINT('Ctrl Pts',(58.1417842183134,-8.27737748783543,-6.69615552976207));
#5213=CARTESIAN_POINT('Ctrl Pts',(58.1653214105115,-8.37098017501116,-6.61712936258409));
#5214=CARTESIAN_POINT('Ctrl Pts',(58.2507030237862,-8.57015853741945,-6.50123578449678));
#5215=CARTESIAN_POINT('Ctrl Pts',(58.3120945049187,-8.67567618723855,-6.46393581086227));
#5216=CARTESIAN_POINT('Ctrl Pts',(58.4186772780868,-8.8337094226362,-6.43126838068827));
#5217=CARTESIAN_POINT('Ctrl Pts',(58.4654152249681,-8.89710038588973,-6.42446144137384));
#5218=CARTESIAN_POINT('Ctrl Pts',(58.5152881956451,-8.9599013972947,-6.42360804569852));
#5219=CARTESIAN_POINT('',(64.5333054217746,-7.98874638935144,-7.59753279036232));
#5220=CARTESIAN_POINT('',(65.0333054217745,-7.98874638935143,-7.59753279036232));
#5221=CARTESIAN_POINT('',(64.5333054217746,-8.9599013972947,-6.42360804569852));
#5222=CARTESIAN_POINT('Ctrl Pts',(64.5333054217746,-8.9599013972947,-6.42360804569852));
#5223=CARTESIAN_POINT('Ctrl Pts',(64.5841440169343,-8.89673206627377,-6.42446644642648));
#5224=CARTESIAN_POINT('Ctrl Pts',(64.6317941862906,-8.83293468780981,-6.43134752238259));
#5225=CARTESIAN_POINT('Ctrl Pts',(64.7397191574786,-8.67483765537062,-6.46423309101336));
#5226=CARTESIAN_POINT('Ctrl Pts',(64.8016959801978,-8.56964482384596,-6.50148776616156));
#5227=CARTESIAN_POINT('Ctrl Pts',(64.8879780992218,-8.37088331138052,-6.61723279487663));
#5228=CARTESIAN_POINT('Ctrl Pts',(64.9118211190309,-8.27737089993273,-6.69616349316846));
#5229=CARTESIAN_POINT('Ctrl Pts',(64.9118211190309,-8.12858066867727,-6.87601998652574));
#5230=CARTESIAN_POINT('Ctrl Pts',(64.8879780992218,-8.06857052864127,-6.98266617408288));
#5231=CARTESIAN_POINT('Ctrl Pts',(64.8016959801978,-7.99211985609405,-7.19959552935062));
#5232=CARTESIAN_POINT('Ctrl Pts',(64.7397191574786,-7.97523623472202,-7.30990593662909));
#5233=CARTESIAN_POINT('Ctrl Pts',(64.6317941862906,-7.9725575896936,-7.47136477705307));
#5234=CARTESIAN_POINT('Ctrl Pts',(64.5841440169343,-7.97775283315432,-7.53532151360656));
#5235=CARTESIAN_POINT('Ctrl Pts',(64.5333054217746,-7.98874638935143,-7.59753279036232));
#5236=CARTESIAN_POINT('',(65.0333054217745,-8.9599013972947,-6.42360804569852));
#5237=CARTESIAN_POINT('Origin',(65.0333054217745,-10.5377236573627,-4.95867635844022));
#5238=CARTESIAN_POINT('',(58.5152881956451,-9.62719480361945,-5.37212188871111));
#5239=CARTESIAN_POINT('',(58.5152881956451,-10.2758959788686,-3.99356171925254));
#5240=CARTESIAN_POINT('Ctrl Pts',(58.5152881956451,-9.62719480361944,-5.37212188871112));
#5241=CARTESIAN_POINT('Ctrl Pts',(58.4654152249681,-9.60122760896735,-5.31493447646361));
#5242=CARTESIAN_POINT('Ctrl Pts',(58.4186772780868,-9.58039615237782,-5.25467836423091));
#5243=CARTESIAN_POINT('Ctrl Pts',(58.3120945049187,-9.54266724792246,-5.09777650237765));
#5244=CARTESIAN_POINT('Ctrl Pts',(58.2507030237862,-9.53149004293564,-4.98641972195919));
#5245=CARTESIAN_POINT('Ctrl Pts',(58.1653214105115,-9.55154766555483,-4.75685266581133));
#5246=CARTESIAN_POINT('Ctrl Pts',(58.1417842183134,-9.5831985936359,-4.63851071679508));
#5247=CARTESIAN_POINT('Ctrl Pts',(58.1417842183134,-9.68259461615746,-4.42728341695521));
#5248=CARTESIAN_POINT('Ctrl Pts',(58.1653214105115,-9.75360359419369,-4.32746196042602));
#5249=CARTESIAN_POINT('Ctrl Pts',(58.2507030237862,-9.91770284122587,-4.16567574773471));
#5250=CARTESIAN_POINT('Ctrl Pts',(58.3120945049187,-10.0106293338081,-4.10330644893437));
#5251=CARTESIAN_POINT('Ctrl Pts',(58.4186772780868,-10.155573604989,-4.03236405867115));
#5252=CARTESIAN_POINT('Ctrl Pts',(58.4654152249681,-10.2152802075941,-4.01000628037358));
#5253=CARTESIAN_POINT('Ctrl Pts',(58.5152881956451,-10.2758959788686,-3.99356171925254));
#5254=CARTESIAN_POINT('',(64.5333054217746,-9.62719480361945,-5.37212188871111));
#5255=CARTESIAN_POINT('',(65.0333054217745,-9.62719480361944,-5.37212188871112));
#5256=CARTESIAN_POINT('',(64.5333054217746,-10.2758959788686,-3.99356171925254));
#5257=CARTESIAN_POINT('Ctrl Pts',(64.5333054217746,-10.2758959788686,-3.99356171925254));
#5258=CARTESIAN_POINT('Ctrl Pts',(64.5841440169343,-10.2149247041221,-4.01010272554701));
#5259=CARTESIAN_POINT('Ctrl Pts',(64.6317941862906,-10.1548428916209,-4.03263338270016));
#5260=CARTESIAN_POINT('Ctrl Pts',(64.7397191574786,-10.009891076528,-4.10380292387847));
#5261=CARTESIAN_POINT('Ctrl Pts',(64.8016959801978,-9.91726793220072,-4.16604756830275));
#5262=CARTESIAN_POINT('Ctrl Pts',(64.8879780992218,-9.75353549627729,-4.32758623220827));
#5263=CARTESIAN_POINT('Ctrl Pts',(64.9118211190309,-9.68259021564447,-4.42729276852132));
#5264=CARTESIAN_POINT('Ctrl Pts',(64.9118211190309,-9.58320299414888,-4.63850136522897));
#5265=CARTESIAN_POINT('Ctrl Pts',(64.8879780992218,-9.55160001136319,-4.75672098164969));
#5266=CARTESIAN_POINT('Ctrl Pts',(64.8016959801978,-9.53149931416127,-4.98584761144596));
#5267=CARTESIAN_POINT('Ctrl Pts',(64.7397191574786,-9.54257920554065,-5.09689120032706));
#5268=CARTESIAN_POINT('Ctrl Pts',(64.6317941862906,-9.58013789587828,-5.25394366630696));
#5269=CARTESIAN_POINT('Ctrl Pts',(64.5841440169343,-9.60107531480922,-5.31459907986337));
#5270=CARTESIAN_POINT('Ctrl Pts',(64.5333054217746,-9.62719480361944,-5.37212188871112));
#5271=CARTESIAN_POINT('',(65.0333054217745,-10.2758959788686,-3.99356171925253));
#5272=CARTESIAN_POINT('Origin',(65.0333054217745,-11.4398343552159,-2.18226511494789));
#5273=CARTESIAN_POINT('',(58.5152881956451,-10.6607311620303,-2.80916081150993));
#5274=CARTESIAN_POINT('',(58.5152881956451,-10.9462182239883,-1.31258522269331));
#5275=CARTESIAN_POINT('Ctrl Pts',(58.5152881956451,-10.6607311620303,-2.80916081150993));
#5276=CARTESIAN_POINT('Ctrl Pts',(58.4654152249681,-10.6213578434494,-2.76022782568649));
#5277=CARTESIAN_POINT('Ctrl Pts',(58.4186772780868,-10.5861957596229,-2.70704534261154));
#5278=CARTESIAN_POINT('Ctrl Pts',(58.3120945049187,-10.5106322717593,-2.56445563826261));
#5279=CARTESIAN_POINT('Ctrl Pts',(58.2507030237862,-10.4721129140633,-2.45937699371878));
#5280=CARTESIAN_POINT('Ctrl Pts',(58.1653214105115,-10.4344493842944,-2.23203408087814));
#5281=CARTESIAN_POINT('Ctrl Pts',(58.1417842183134,-10.4356754943201,-2.10953879607271));
#5282=CARTESIAN_POINT('Ctrl Pts',(58.1417842183134,-10.4794187146543,-1.88022880465162));
#5283=CARTESIAN_POINT('Ctrl Pts',(58.1653214105115,-10.5233722283083,-1.76588420800258));
#5284=CARTESIAN_POINT('Ctrl Pts',(58.2507030237862,-10.6420814007585,-1.56837098345874));
#5285=CARTESIAN_POINT('Ctrl Pts',(58.3120945049187,-10.7165778228152,-1.48485125191443));
#5286=CARTESIAN_POINT('Ctrl Pts',(58.4186772780868,-10.8393257481533,-1.38009147285009));
#5287=CARTESIAN_POINT('Ctrl Pts',(58.4654152249681,-10.8915964046827,-1.34358767700596));
#5288=CARTESIAN_POINT('Ctrl Pts',(58.5152881956451,-10.9462182239883,-1.31258522269331));
#5289=CARTESIAN_POINT('',(64.5333054217746,-10.6607311620303,-2.80916081150993));
#5290=CARTESIAN_POINT('',(65.0333054217746,-10.6607311620303,-2.80916081150993));
#5291=CARTESIAN_POINT('',(64.5333054217746,-10.9462182239883,-1.31258522269331));
#5292=CARTESIAN_POINT('Ctrl Pts',(64.5333054217746,-10.9462182239883,-1.31258522269331));
#5293=CARTESIAN_POINT('Ctrl Pts',(64.5841440169343,-10.8912760549453,-1.34376950229525));
#5294=CARTESIAN_POINT('Ctrl Pts',(64.6317941862906,-10.8386849696517,-1.38053405659456));
#5295=CARTESIAN_POINT('Ctrl Pts',(64.7397191574786,-10.7159862275429,-1.4855157263049));
#5296=CARTESIAN_POINT('Ctrl Pts',(64.8016959801978,-10.6417526232152,-1.5688392800763));
#5297=CARTESIAN_POINT('Ctrl Pts',(64.8879780992218,-10.5233371749486,-1.76602151082142));
#5298=CARTESIAN_POINT('Ctrl Pts',(64.9118211190309,-10.4794167780314,-1.88023895678416));
#5299=CARTESIAN_POINT('Ctrl Pts',(64.9118211190309,-10.4356774309429,-2.10952864394017));
#5300=CARTESIAN_POINT('Ctrl Pts',(64.8879780992218,-10.4344673370436,-2.23189351594341));
#5301=CARTESIAN_POINT('Ctrl Pts',(64.8016959801978,-10.4719796159174,-2.45882055144931));
#5302=CARTESIAN_POINT('Ctrl Pts',(64.7397191574786,-10.5103268297238,-2.5636200448539));
#5303=CARTESIAN_POINT('Ctrl Pts',(64.6317941862906,-10.5857629047824,-2.70639795235363));
#5304=CARTESIAN_POINT('Ctrl Pts',(64.5841440169343,-10.6211269241497,-2.75994084020421));
#5305=CARTESIAN_POINT('Ctrl Pts',(64.5333054217746,-10.6607311620303,-2.80916081150993));
#5306=CARTESIAN_POINT('',(65.0333054217746,-10.9462182239883,-1.31258522269331));
#5307=CARTESIAN_POINT('Origin',(65.0333054217745,-11.6231381877631,0.731265871526303));
#5308=CARTESIAN_POINT('',(58.5152881956451,-11.0244145741041,-0.0696898291507972));
#5309=CARTESIAN_POINT('',(58.5152881956451,-10.9287493207203,1.45086583075851));
#5310=CARTESIAN_POINT('Ctrl Pts',(58.5152881956451,-11.0244145741041,-0.0696898291508038));
#5311=CARTESIAN_POINT('Ctrl Pts',(58.4654152249681,-10.9741091020059,-0.0320859092136465));
#5312=CARTESIAN_POINT('Ctrl Pts',(58.4186772780868,-10.9268257539862,0.0106812937004472));
#5313=CARTESIAN_POINT('Ctrl Pts',(58.3120945049187,-10.8181756145601,0.129999405012571));
#5314=CARTESIAN_POINT('Ctrl Pts',(58.2507030237862,-10.7547344170632,0.22219743599286));
#5315=CARTESIAN_POINT('Ctrl Pts',(58.1653214105115,-10.6617162729982,0.433031414203767));
#5316=CARTESIAN_POINT('Ctrl Pts',(58.1417842183134,-10.6324405239663,0.551983205547908));
#5317=CARTESIAN_POINT('Ctrl Pts',(58.1417842183134,-10.6177823947033,0.784967498446072));
#5318=CARTESIAN_POINT('Ctrl Pts',(58.1653214105115,-10.6319186830624,0.906650543677475));
#5319=CARTESIAN_POINT('Ctrl Pts',(58.2507030237862,-10.6977788470438,1.12748029777295));
#5320=CARTESIAN_POINT('Ctrl Pts',(58.3120945049187,-10.7491643143985,1.22690261016421));
#5321=CARTESIAN_POINT('Ctrl Pts',(58.4186772780868,-10.8420031903095,1.35889733583154));
#5322=CARTESIAN_POINT('Ctrl Pts',(58.4654152249681,-10.8835535431755,1.40725348147776));
#5323=CARTESIAN_POINT('Ctrl Pts',(58.5152881956451,-10.9287493207203,1.45086583075852));
#5324=CARTESIAN_POINT('',(64.5333054217746,-11.0244145741041,-0.0696898291507972));
#5325=CARTESIAN_POINT('',(65.0333054217745,-11.0244145741041,-0.0696898291508069));
#5326=CARTESIAN_POINT('',(64.5333054217746,-10.9287493207203,1.45086583075851));
#5327=CARTESIAN_POINT('Ctrl Pts',(64.5333054217746,-10.9287493207203,1.45086583075851));
#5328=CARTESIAN_POINT('Ctrl Pts',(64.5841440169343,-10.8832884759249,1.40699770082426));
#5329=CARTESIAN_POINT('Ctrl Pts',(64.6317941862906,-10.8414926091443,1.35830930153599));
#5330=CARTESIAN_POINT('Ctrl Pts',(64.7397191574786,-10.7487565532408,1.22611188769709));
#5331=CARTESIAN_POINT('Ctrl Pts',(64.8016959801978,-10.6975768592847,1.12694494990463));
#5332=CARTESIAN_POINT('Ctrl Pts',(64.8879780992218,-10.6319188767911,0.906508837063125));
#5333=CARTESIAN_POINT('Ctrl Pts',(64.911821119031,-10.6177830436557,0.784957183642927));
#5334=CARTESIAN_POINT('Ctrl Pts',(64.911821119031,-10.6324398750139,0.551993520351054));
#5335=CARTESIAN_POINT('Ctrl Pts',(64.8879780992218,-10.6616987046511,0.433172027699774));
#5336=CARTESIAN_POINT('Ctrl Pts',(64.8016959801978,-10.7544669251584,0.222703246704335));
#5337=CARTESIAN_POINT('Ctrl Pts',(64.7397191574786,-10.8176719649172,0.130732786372442));
#5338=CARTESIAN_POINT('Ctrl Pts',(64.6317941862906,-10.9262454986663,0.0112006983815039));
#5339=CARTESIAN_POINT('Ctrl Pts',(64.5841440169343,-10.9738140670733,-0.0318653672026201));
#5340=CARTESIAN_POINT('Ctrl Pts',(64.5333054217746,-11.0244145741041,-0.0696898291508038));
#5341=CARTESIAN_POINT('',(65.0333054217745,-10.9287493207203,1.45086583075852));
#5342=CARTESIAN_POINT('Origin',(65.0333054217745,-11.0761175010611,3.59884873388475));
#5343=CARTESIAN_POINT('',(58.5152881956451,-10.6953934735264,2.67416002147514));
#5344=CARTESIAN_POINT('',(58.5152881956451,-10.2245869045029,4.1231536481525));
#5345=CARTESIAN_POINT('Ctrl Pts',(58.5152881956451,-10.6953934735264,2.67416002147514));
#5346=CARTESIAN_POINT('Ctrl Pts',(58.4654152249681,-10.6373167257333,2.69807208293881));
#5347=CARTESIAN_POINT('Ctrl Pts',(58.4186772780868,-10.5808831001726,2.72773678504619));
#5348=CARTESIAN_POINT('Ctrl Pts',(58.3120945049187,-10.4459731970312,2.81628610756645));
#5349=CARTESIAN_POINT('Ctrl Pts',(58.2507030237862,-10.3615964034925,2.88981038361606));
#5350=CARTESIAN_POINT('Ctrl Pts',(58.1653214105115,-10.21906831722,3.07088795295311));
#5351=CARTESIAN_POINT('Ctrl Pts',(58.1417842183134,-10.1611302121108,3.17882207231172));
#5352=CARTESIAN_POINT('Ctrl Pts',(58.1417842183134,-10.088991757421,3.40084140670788));
#5353=CARTESIAN_POINT('Ctrl Pts',(58.1653214105115,-10.072422585498,3.52221710727082));
#5354=CARTESIAN_POINT('Ctrl Pts',(58.2507030237862,-10.081295504691,3.75248784531307));
#5355=CARTESIAN_POINT('Ctrl Pts',(58.3120945049187,-10.1063412794472,3.86156566901407));
#5356=CARTESIAN_POINT('Ctrl Pts',(58.4186772780868,-10.1634376979201,4.01250162722806));
#5357=CARTESIAN_POINT('Ctrl Pts',(58.4654152249681,-10.1916569856406,4.06967172820396));
#5358=CARTESIAN_POINT('Ctrl Pts',(58.5152881956451,-10.2245869045029,4.12315364815251));
#5359=CARTESIAN_POINT('',(64.5333054217746,-10.6953934735264,2.67416002147514));
#5360=CARTESIAN_POINT('',(65.0333054217745,-10.6953934735264,2.67416002147513));
#5361=CARTESIAN_POINT('',(64.5333054217746,-10.2245869045029,4.1231536481525));
#5362=CARTESIAN_POINT('Ctrl Pts',(64.5333054217746,-10.2245869045029,4.12315364815251));
#5363=CARTESIAN_POINT('Ctrl Pts',(64.5841440169343,-10.1914638560269,4.06935806382539));
#5364=CARTESIAN_POINT('Ctrl Pts',(64.6317941862906,-10.1630893957837,4.01180509073887));
#5365=CARTESIAN_POINT('Ctrl Pts',(64.7397191574786,-10.1061429735371,3.86069838247098));
#5366=CARTESIAN_POINT('Ctrl Pts',(64.8016959801978,-10.0812329983496,3.75191908406943));
#5367=CARTESIAN_POINT('Ctrl Pts',(64.8879780992218,-10.0724580141423,3.5220799008087));
#5368=CARTESIAN_POINT('Ctrl Pts',(64.9118211190309,-10.0889949511726,3.40083157735114));
#5369=CARTESIAN_POINT('Ctrl Pts',(64.9118211190309,-10.1611270183592,3.17883190166846));
#5370=CARTESIAN_POINT('Ctrl Pts',(64.8879780992218,-10.2190163316603,3.0710197797473));
#5371=CARTESIAN_POINT('Ctrl Pts',(64.8016959801978,-10.3612115253291,2.8902337808223));
#5372=CARTESIAN_POINT('Ctrl Pts',(64.7397191574786,-10.4453029859404,2.81687119582945));
#5373=CARTESIAN_POINT('Ctrl Pts',(64.6317941862906,-10.580191903949,2.72809556804404));
#5374=CARTESIAN_POINT('Ctrl Pts',(64.5841440169343,-10.6369761132978,2.69821232401293));
#5375=CARTESIAN_POINT('Ctrl Pts',(64.5333054217746,-10.6953934735264,2.67416002147514));
#5376=CARTESIAN_POINT('',(65.0333054217745,-10.2245869045029,4.12315364815251));
#5377=CARTESIAN_POINT('Origin',(65.0333054217745,-9.83314361665672,6.24030269465341));
#5378=CARTESIAN_POINT('',(58.5152881956451,-9.69434146610128,5.2499825630792));
#5379=CARTESIAN_POINT('',(58.5152881956451,-8.87797608967546,6.53636855793469));
#5380=CARTESIAN_POINT('Ctrl Pts',(58.5152881956451,-9.69434146610128,5.24998256307919));
#5381=CARTESIAN_POINT('Ctrl Pts',(58.4654152249681,-9.63214261826849,5.25870028330521));
#5382=CARTESIAN_POINT('Ctrl Pts',(58.4186772780868,-9.57010464740912,5.27339854227333));
#5383=CARTESIAN_POINT('Ctrl Pts',(58.3120945049187,-9.41741186593077,5.32561519640614));
#5384=CARTESIAN_POINT('Ctrl Pts',(58.2507030237862,-9.31740118060456,5.37584591685751));
#5385=CARTESIAN_POINT('Ctrl Pts',(58.1653214105115,-9.13431871596657,5.51578930768254));
#5386=CARTESIAN_POINT('Ctrl Pts',(58.1417842183134,-9.05135871900561,5.60592385738239));
#5387=CARTESIAN_POINT('Ctrl Pts',(58.1417842183134,-8.9262726633038,5.80302794196643));
#5388=CARTESIAN_POINT('Ctrl Pts',(58.1653214105115,-8.88003913310781,5.91646981620596));
#5389=CARTESIAN_POINT('Ctrl Pts',(58.2507030237862,-8.83136728936705,6.14171278084726));
#5390=CARTESIAN_POINT('Ctrl Pts',(58.3120945049187,-8.82849965338492,6.25359235503467));
#5391=CARTESIAN_POINT('Ctrl Pts',(58.4186772780868,-8.84626603646125,6.41398568443713));
#5392=CARTESIAN_POINT('Ctrl Pts',(58.4654152249681,-8.85938113740538,6.47637753304146));
#5393=CARTESIAN_POINT('Ctrl Pts',(58.5152881956451,-8.87797608967545,6.53636855793469));
#5394=CARTESIAN_POINT('',(64.5333054217746,-9.69434146610128,5.2499825630792));
#5395=CARTESIAN_POINT('',(65.0333054217745,-9.69434146610129,5.24998256307919));
#5396=CARTESIAN_POINT('',(64.5333054217746,-8.87797608967546,6.53636855793469));
#5397=CARTESIAN_POINT('Ctrl Pts',(64.5333054217746,-8.87797608967545,6.53636855793469));
#5398=CARTESIAN_POINT('Ctrl Pts',(64.5841440169343,-8.85927208047261,6.47602569362432));
#5399=CARTESIAN_POINT('Ctrl Pts',(64.6317941862906,-8.84610189845785,6.41322441170358));
#5400=CARTESIAN_POINT('Ctrl Pts',(64.7397191574786,-8.82852326301227,6.25270299921878));
#5401=CARTESIAN_POINT('Ctrl Pts',(64.8016959801978,-8.83144819194687,6.14114634358899));
#5402=CARTESIAN_POINT('Ctrl Pts',(64.8879780992218,-8.88010757055562,5.91634573108268));
#5403=CARTESIAN_POINT('Ctrl Pts',(64.9118211190309,-8.92627820117944,5.80301921567074));
#5404=CARTESIAN_POINT('Ctrl Pts',(64.9118211190309,-9.05135318112997,5.60593258367809));
#5405=CARTESIAN_POINT('Ctrl Pts',(64.8879780992218,-9.13423557963828,5.5159040646126));
#5406=CARTESIAN_POINT('Ctrl Pts',(64.8016959801978,-9.31692309949288,5.37616029695489));
#5407=CARTESIAN_POINT('Ctrl Pts',(64.7397191574786,-9.41661720521969,5.3260152283249));
#5408=CARTESIAN_POINT('Ctrl Pts',(64.6317941862906,-9.5693459406827,5.2735741599327));
#5409=CARTESIAN_POINT('Ctrl Pts',(64.5841440169343,-9.63177783026215,5.25875141157996));
#5410=CARTESIAN_POINT('Ctrl Pts',(64.5333054217746,-9.69434146610128,5.24998256307919));
#5411=CARTESIAN_POINT('',(65.0333054217745,-8.87797608967545,6.5363685579347));
#5412=CARTESIAN_POINT('Origin',(65.0333054217745,-7.97231715504529,8.48965548688909));
#5413=CARTESIAN_POINT('',(58.5152881956451,-8.08415833106712,7.49592939215974));
#5414=CARTESIAN_POINT('',(58.5152881956451,-6.97352938622158,8.53887939213984));
#5415=CARTESIAN_POINT('Ctrl Pts',(58.5152881956451,-8.08415833106713,7.49592939215973));
#5416=CARTESIAN_POINT('Ctrl Pts',(58.4654152249681,-8.02174556555534,7.48890500472477));
#5417=CARTESIAN_POINT('Ctrl Pts',(58.4186772780868,-7.95800132326607,7.48771327488624));
#5418=CARTESIAN_POINT('Ctrl Pts',(58.3120945049187,-7.79711991247583,7.50031629621302));
#5419=CARTESIAN_POINT('Ctrl Pts',(58.2507030237862,-7.68775937453467,7.52409728016453));
#5420=CARTESIAN_POINT('Ctrl Pts',(58.1653214105115,-7.47562627611464,7.6141133345562));
#5421=CARTESIAN_POINT('Ctrl Pts',(58.1417842183134,-7.37285706901645,7.68078482934798));
#5422=CARTESIAN_POINT('Ctrl Pts',(58.1417842183134,-7.20268302921675,7.84058888958737));
#5423=CARTESIAN_POINT('Ctrl Pts',(58.1653214105115,-7.12969016348498,7.93896896733497));
#5424=CARTESIAN_POINT('Ctrl Pts',(58.2507030237862,-7.02653178775528,8.14503131472123));
#5425=CARTESIAN_POINT('Ctrl Pts',(58.3120945049187,-6.99593092515002,8.25268283428457));
#5426=CARTESIAN_POINT('Ctrl Pts',(58.4186772780868,-6.97325094564082,8.41245543210373));
#5427=CARTESIAN_POINT('Ctrl Pts',(58.4654152249681,-6.97043778978239,8.47614871902753));
#5428=CARTESIAN_POINT('Ctrl Pts',(58.5152881956451,-6.97352938622157,8.53887939213984));
#5429=CARTESIAN_POINT('',(64.5333054217746,-8.08415833106712,7.49592939215974));
#5430=CARTESIAN_POINT('',(65.0333054217745,-8.08415833106713,7.49592939215973));
#5431=CARTESIAN_POINT('',(64.5333054217746,-6.97352938622158,8.53887939213984));
#5432=CARTESIAN_POINT('Ctrl Pts',(64.5333054217746,-6.97352938622157,8.53887939213984));
#5433=CARTESIAN_POINT('Ctrl Pts',(64.5841440169343,-6.97041965797865,8.47578081193636));
#5434=CARTESIAN_POINT('Ctrl Pts',(64.6317941862906,-6.97328128516483,8.41167725669145));
#5435=CARTESIAN_POINT('Ctrl Pts',(64.7397191574786,-6.99617496683501,8.25182729069261));
#5436=CARTESIAN_POINT('Ctrl Pts',(64.8016959801978,-7.02675101584963,8.14450279278449));
#5437=CARTESIAN_POINT('Ctrl Pts',(64.8879780992218,-7.12978730955983,7.9388658002752));
#5438=CARTESIAN_POINT('Ctrl Pts',(64.9118211190309,-7.20269056325133,7.84058181465797));
#5439=CARTESIAN_POINT('Ctrl Pts',(64.9118211190309,-7.37284953498187,7.68079190427738));
#5440=CARTESIAN_POINT('Ctrl Pts',(64.8879780992218,-7.47551721277898,7.61420381102219));
#5441=CARTESIAN_POINT('Ctrl Pts',(64.8016959801978,-7.68721813006929,7.52428288949532));
#5442=CARTESIAN_POINT('Ctrl Pts',(64.7397191574786,-7.79625073359953,7.50050613631087));
#5443=CARTESIAN_POINT('Ctrl Pts',(64.6317941862906,-7.95722277837073,7.48769469250372));
#5444=CARTESIAN_POINT('Ctrl Pts',(64.5841440169343,-8.02137952295014,7.48886380762261));
#5445=CARTESIAN_POINT('Ctrl Pts',(64.5333054217746,-8.08415833106713,7.49592939215973));
#5446=CARTESIAN_POINT('',(65.0333054217745,-6.97352938622157,8.53887939213985));
#5447=CARTESIAN_POINT('Origin',(65.0333054217745,-5.61056068645084,10.2055720021147));
#5448=CARTESIAN_POINT('',(58.5152881956451,-5.96601779663743,9.270879409431));
#5449=CARTESIAN_POINT('',(58.5152881956451,-4.63091018458434,10.0048610303352));
#5450=CARTESIAN_POINT('Ctrl Pts',(58.5152881956451,-5.96601779663743,9.270879409431));
#5451=CARTESIAN_POINT('Ctrl Pts',(58.4654152249681,-5.90731273704185,9.24855428243148));
#5452=CARTESIAN_POINT('Ctrl Pts',(58.4186772780868,-5.84586750850063,9.23154744455494));
#5453=CARTESIAN_POINT('Ctrl Pts',(58.3120945049187,-5.6869062391189,9.20374493889505));
#5454=CARTESIAN_POINT('Ctrl Pts',(58.2507030237862,-5.57506737336155,9.19958193966467));
#5455=CARTESIAN_POINT('Ctrl Pts',(58.1653214105115,-5.34721274390418,9.23401461786969));
#5456=CARTESIAN_POINT('Ctrl Pts',(58.1417842183134,-5.23109169390945,9.273033842535));
#5457=CARTESIAN_POINT('Ctrl Pts',(58.1417842183134,-5.0265223307888,9.38549680160669));
#5458=CARTESIAN_POINT('Ctrl Pts',(58.1653214105115,-4.93135653972418,9.46263350076087));
#5459=CARTESIAN_POINT('Ctrl Pts',(58.2507030237862,-4.78019345214259,9.63656757576151));
#5460=CARTESIAN_POINT('Ctrl Pts',(58.3120945049187,-4.72378212765379,9.73322689981202));
#5461=CARTESIAN_POINT('Ctrl Pts',(58.4186772780868,-4.66208085208275,9.88233966612439));
#5462=CARTESIAN_POINT('Ctrl Pts',(58.4654152249681,-4.64351620035041,9.9433323079027));
#5463=CARTESIAN_POINT('Ctrl Pts',(58.5152881956451,-4.63091018458433,10.0048610303352));
#5464=CARTESIAN_POINT('',(64.5333054217746,-5.96601779663743,9.270879409431));
#5465=CARTESIAN_POINT('',(65.0333054217745,-5.96601779663744,9.270879409431));
#5466=CARTESIAN_POINT('',(64.5333054217746,-4.63091018458434,10.0048610303352));
#5467=CARTESIAN_POINT('Ctrl Pts',(64.5333054217746,-4.63091018458433,10.0048610303352));
#5468=CARTESIAN_POINT('Ctrl Pts',(64.5841440169343,-4.64359013296362,9.94297145009311));
#5469=CARTESIAN_POINT('Ctrl Pts',(64.6317941862906,-4.66230376279031,9.88159348365645));
#5470=CARTESIAN_POINT('Ctrl Pts',(64.7397191574786,-4.72423126735984,9.73245892539434));
#5471=CARTESIAN_POINT('Ctrl Pts',(64.8016959801978,-4.78053723084403,9.63611017812334));
#5472=CARTESIAN_POINT('Ctrl Pts',(64.8879780992218,-4.9314762903809,9.46255773413038));
#5473=CARTESIAN_POINT('Ctrl Pts',(64.9118211190309,-5.02653138759124,9.38549182258742));
#5474=CARTESIAN_POINT('Ctrl Pts',(64.9118211190309,-5.23108263710702,9.27303882155427));
#5475=CARTESIAN_POINT('Ctrl Pts',(64.8879780992218,-5.34708460641165,9.23407512890247));
#5476=CARTESIAN_POINT('Ctrl Pts',(64.8016959801978,-5.5744969739228,9.19962711571201));
#5477=CARTESIAN_POINT('Ctrl Pts',(64.7397191574786,-5.68601715578279,9.20371265882047));
#5478=CARTESIAN_POINT('Ctrl Pts',(64.6317941862906,-5.84511804427543,9.23133582972995));
#5479=CARTESIAN_POINT('Ctrl Pts',(64.5841440169343,-5.90696843964088,9.24842334851785));
#5480=CARTESIAN_POINT('Ctrl Pts',(64.5333054217746,-5.96601779663743,9.270879409431));
#5481=CARTESIAN_POINT('',(65.0333054217745,-4.63091018458433,10.0048610303352));
#5482=CARTESIAN_POINT('Origin',(65.0333054217745,-2.89627205572787,11.2802348949791));
#5483=CARTESIAN_POINT('',(58.5152881956451,-3.47301042256638,10.4633059774983));
#5484=CARTESIAN_POINT('',(58.5152881956451,-1.99731386475336,10.8422004546895));
#5485=CARTESIAN_POINT('Ctrl Pts',(58.5152881956451,-3.47301042256638,10.4633059774983));
#5486=CARTESIAN_POINT('Ctrl Pts',(58.4654152249681,-3.4217017236835,10.4270828807697));
#5487=CARTESIAN_POINT('Ctrl Pts',(58.4186772780868,-3.36641633857933,10.3953295370257));
#5488=CARTESIAN_POINT('Ctrl Pts',(58.3120945049187,-3.21936333178,10.3288684380602));
#5489=CARTESIAN_POINT('Ctrl Pts',(58.2507030237862,-3.11207338545658,10.2970230322));
#5490=CARTESIAN_POINT('Ctrl Pts',(58.1653214105115,-2.88281416932138,10.2737088024122));
#5491=CARTESIAN_POINT('Ctrl Pts',(58.1417842183134,-2.76063758906464,10.2826240355627));
#5492=CARTESIAN_POINT('Ctrl Pts',(58.1417842183134,-2.5345267480614,10.3406794321384));
#5493=CARTESIAN_POINT('Ctrl Pts',(58.1653214105115,-2.4231676483118,10.3917259702023));
#5494=CARTESIAN_POINT('Ctrl Pts',(58.2507030237862,-2.23349798161003,10.5226028552003));
#5495=CARTESIAN_POINT('Ctrl Pts',(58.3120945049187,-2.15482072622166,10.6021965229197));
#5496=CARTESIAN_POINT('Ctrl Pts',(58.4186772780868,-2.05797507265433,10.7312801542195));
#5497=CARTESIAN_POINT('Ctrl Pts',(58.4654152249681,-2.02482541039243,10.7857397588542));
#5498=CARTESIAN_POINT('Ctrl Pts',(58.5152881956451,-1.99731386475336,10.8422004546895));
#5499=CARTESIAN_POINT('',(64.5333054217746,-3.47301042256638,10.4633059774983));
#5500=CARTESIAN_POINT('',(65.0333054217745,-3.47301042256639,10.4633059774983));
#5501=CARTESIAN_POINT('',(64.5333054217746,-1.99731386475336,10.8422004546895));
#5502=CARTESIAN_POINT('Ctrl Pts',(64.5333054217746,-1.99731386475336,10.8422004546895));
#5503=CARTESIAN_POINT('Ctrl Pts',(64.5841440169343,-2.0249867619646,10.7854086243495));
#5504=CARTESIAN_POINT('Ctrl Pts',(64.6317941862906,-2.05837654824586,10.7306128500846));
#5505=CARTESIAN_POINT('Ctrl Pts',(64.7397191574786,-2.15544674284921,10.6015643723334));
#5506=CARTESIAN_POINT('Ctrl Pts',(64.8016959801978,-2.23394471003843,10.5222453218365));
#5507=CARTESIAN_POINT('Ctrl Pts',(64.8879780992218,-2.42330247917622,10.3916823646972));
#5508=CARTESIAN_POINT('Ctrl Pts',(64.9118211190309,-2.53453675855947,10.3406768618793));
#5509=CARTESIAN_POINT('Ctrl Pts',(64.9118211190309,-2.76062757856657,10.2826266058217));
#5510=CARTESIAN_POINT('Ctrl Pts',(64.8879780992218,-2.88267500902189,10.2737355458811));
#5511=CARTESIAN_POINT('Ctrl Pts',(64.8016959801978,-3.11150967133898,10.2969249363867));
#5512=CARTESIAN_POINT('Ctrl Pts',(64.7397191574786,-3.21851020835992,10.328616066089));
#5513=CARTESIAN_POINT('Ctrl Pts',(64.6317941862906,-3.36574304661788,10.3949381862959));
#5514=CARTESIAN_POINT('Ctrl Pts',(64.5841440169343,-3.42140080495871,10.4268704371039));
#5515=CARTESIAN_POINT('Ctrl Pts',(64.5333054217746,-3.47301042256638,10.4633059774983));
#5516=CARTESIAN_POINT('',(65.0333054217745,-1.99731386475336,10.8422004546896));
#5517=CARTESIAN_POINT('Origin',(64.7833054217745,0.,0.));
#5518=CARTESIAN_POINT('',(65.0333054217745,-1.28889603700374E-15,10.5246348408465));
#5519=CARTESIAN_POINT('Origin',(65.0333054217745,0.,0.));
#5520=CARTESIAN_POINT('',(64.911821119031,-7.73317429945324E-16,10.6461191435901));
#5521=CARTESIAN_POINT('',(64.7833054217745,-1.31951220698242E-15,10.7746348408465));
#5522=CARTESIAN_POINT('',(64.5333054217746,-0.761781030806626,10.9982845496518));
#5523=CARTESIAN_POINT('Ctrl Pts',(64.911821119031,-2.60208521396521E-16,
10.6461191435901));
#5524=CARTESIAN_POINT('Ctrl Pts',(64.911821119031,-0.116712136386744,10.6461191435901));
#5525=CARTESIAN_POINT('Ctrl Pts',(64.8879780992218,-0.237136339078202,10.6678593743557));
#5526=CARTESIAN_POINT('Ctrl Pts',(64.8016959801978,-0.453014772772831,10.7472290938673));
#5527=CARTESIAN_POINT('Ctrl Pts',(64.7397191574786,-0.548772427693239,10.8045345399324));
#5528=CARTESIAN_POINT('Ctrl Pts',(64.6317941862906,-0.674886035004275,10.9053883467085));
#5529=CARTESIAN_POINT('Ctrl Pts',(64.5841440169343,-0.720853974669018,10.9501589087797));
#5530=CARTESIAN_POINT('Ctrl Pts',(64.5333054217746,-0.761781030806632,10.9982845496518));
#5531=CARTESIAN_POINT('Origin',(64.5333054217746,0.,0.));
#5532=CARTESIAN_POINT('Origin',(64.5333054217746,0.,0.));
#5533=CARTESIAN_POINT('Origin',(64.5333054217746,0.,0.));
#5534=CARTESIAN_POINT('Origin',(64.5333054217746,0.,0.));
#5535=CARTESIAN_POINT('Origin',(64.5333054217746,0.,0.));
#5536=CARTESIAN_POINT('Origin',(64.5333054217746,0.,0.));
#5537=CARTESIAN_POINT('Origin',(64.5333054217746,0.,0.));
#5538=CARTESIAN_POINT('Origin',(64.5333054217746,0.,0.));
#5539=CARTESIAN_POINT('Origin',(64.5333054217746,0.,0.));
#5540=CARTESIAN_POINT('Origin',(64.5333054217746,0.,0.));
#5541=CARTESIAN_POINT('Origin',(64.5333054217746,0.,0.));
#5542=CARTESIAN_POINT('Origin',(64.5333054217746,0.,0.));
#5543=CARTESIAN_POINT('Origin',(64.5333054217746,0.,0.));
#5544=CARTESIAN_POINT('Origin',(64.5333054217746,0.,0.));
#5545=CARTESIAN_POINT('Origin',(64.5333054217746,0.,0.));
#5546=CARTESIAN_POINT('Origin',(64.5333054217746,0.,0.));
#5547=CARTESIAN_POINT('Origin',(64.5333054217746,0.,0.));
#5548=CARTESIAN_POINT('Origin',(64.5333054217746,0.,0.));
#5549=CARTESIAN_POINT('Origin',(64.5333054217746,0.,0.));
#5550=CARTESIAN_POINT('Origin',(64.5333054217746,0.,0.));
#5551=CARTESIAN_POINT('Origin',(64.5333054217746,0.,0.));
#5552=CARTESIAN_POINT('Origin',(64.5333054217746,0.,0.));
#5553=CARTESIAN_POINT('Origin',(64.5333054217746,0.,0.));
#5554=CARTESIAN_POINT('Origin',(64.5333054217746,0.,0.));
#5555=CARTESIAN_POINT('',(64.5333054217746,0.761781030806626,10.9982845496518));
#5556=CARTESIAN_POINT('Origin',(64.5333054217746,0.,0.));
#5557=CARTESIAN_POINT('Ctrl Pts',(64.5333054217746,0.761781030806632,10.9982845496518));
#5558=CARTESIAN_POINT('Ctrl Pts',(64.5841440169343,0.720853974669017,10.9501589087797));
#5559=CARTESIAN_POINT('Ctrl Pts',(64.6317941862906,0.674886035004276,10.9053883467085));
#5560=CARTESIAN_POINT('Ctrl Pts',(64.7397191574786,0.548772427693241,10.8045345399324));
#5561=CARTESIAN_POINT('Ctrl Pts',(64.8016959801978,0.453014772772831,10.7472290938673));
#5562=CARTESIAN_POINT('Ctrl Pts',(64.8879780992218,0.237136339078202,10.6678593743557));
#5563=CARTESIAN_POINT('Ctrl Pts',(64.911821119031,0.116712136386744,10.6461191435901));
#5564=CARTESIAN_POINT('Ctrl Pts',(64.911821119031,7.97972798949331E-16,
10.6461191435901));
#5565=CARTESIAN_POINT('Origin',(61.5242968087098,0.,0.));
#5566=CARTESIAN_POINT('',(58.5152881956451,0.761781030806626,10.9982845496518));
#5567=CARTESIAN_POINT('Origin',(58.5152881956451,0.,0.));
#5568=CARTESIAN_POINT('',(65.0333054217745,0.761781030806634,10.9982845496518));
#5569=CARTESIAN_POINT('Origin',(61.5242968087098,0.,0.));
#5570=CARTESIAN_POINT('',(58.5152881956451,-0.761781030806626,10.9982845496518));
#5571=CARTESIAN_POINT('',(65.0333054217745,-0.761781030806634,10.9982845496518));
#5572=CARTESIAN_POINT('Origin',(58.5152881956451,0.,0.));
#5573=CARTESIAN_POINT('Origin',(61.5242968087098,0.,0.));
#5574=CARTESIAN_POINT('Origin',(58.5152881956451,0.,0.));
#5575=CARTESIAN_POINT('Origin',(61.5242968087098,0.,0.));
#5576=CARTESIAN_POINT('Origin',(58.5152881956451,0.,0.));
#5577=CARTESIAN_POINT('Origin',(61.5242968087098,0.,0.));
#5578=CARTESIAN_POINT('Origin',(58.5152881956451,0.,0.));
#5579=CARTESIAN_POINT('Origin',(61.5242968087098,0.,0.));
#5580=CARTESIAN_POINT('Origin',(58.5152881956451,0.,0.));
#5581=CARTESIAN_POINT('Origin',(61.5242968087098,0.,0.));
#5582=CARTESIAN_POINT('Origin',(58.5152881956451,0.,0.));
#5583=CARTESIAN_POINT('Origin',(61.5242968087098,0.,0.));
#5584=CARTESIAN_POINT('Origin',(58.5152881956451,0.,0.));
#5585=CARTESIAN_POINT('Origin',(61.5242968087098,0.,0.));
#5586=CARTESIAN_POINT('Origin',(58.5152881956451,0.,0.));
#5587=CARTESIAN_POINT('Origin',(61.5242968087098,0.,0.));
#5588=CARTESIAN_POINT('Origin',(58.5152881956451,0.,0.));
#5589=CARTESIAN_POINT('Origin',(61.5242968087098,0.,0.));
#5590=CARTESIAN_POINT('Origin',(58.5152881956451,0.,0.));
#5591=CARTESIAN_POINT('Origin',(61.5242968087098,0.,0.));
#5592=CARTESIAN_POINT('Origin',(58.5152881956451,0.,0.));
#5593=CARTESIAN_POINT('Origin',(61.5242968087098,0.,0.));
#5594=CARTESIAN_POINT('Origin',(58.5152881956451,0.,0.));
#5595=CARTESIAN_POINT('Origin',(61.5242968087098,0.,0.));
#5596=CARTESIAN_POINT('Origin',(58.5152881956451,0.,0.));
#5597=CARTESIAN_POINT('Origin',(61.5242968087098,0.,0.));
#5598=CARTESIAN_POINT('Origin',(58.5152881956451,0.,0.));
#5599=CARTESIAN_POINT('Origin',(61.5242968087098,0.,0.));
#5600=CARTESIAN_POINT('Origin',(58.5152881956451,0.,0.));
#5601=CARTESIAN_POINT('Origin',(61.5242968087098,0.,0.));
#5602=CARTESIAN_POINT('Origin',(58.5152881956451,0.,0.));
#5603=CARTESIAN_POINT('Origin',(61.5242968087098,0.,0.));
#5604=CARTESIAN_POINT('Origin',(58.5152881956451,0.,0.));
#5605=CARTESIAN_POINT('Origin',(61.5242968087098,0.,0.));
#5606=CARTESIAN_POINT('Origin',(58.5152881956451,0.,0.));
#5607=CARTESIAN_POINT('Origin',(61.5242968087098,0.,0.));
#5608=CARTESIAN_POINT('Origin',(58.5152881956451,0.,0.));
#5609=CARTESIAN_POINT('Origin',(61.5242968087098,0.,0.));
#5610=CARTESIAN_POINT('Origin',(58.5152881956451,0.,0.));
#5611=CARTESIAN_POINT('Origin',(61.5242968087098,0.,0.));
#5612=CARTESIAN_POINT('Origin',(58.5152881956451,0.,0.));
#5613=CARTESIAN_POINT('Origin',(61.5242968087098,0.,0.));
#5614=CARTESIAN_POINT('Origin',(58.5152881956451,0.,0.));
#5615=CARTESIAN_POINT('Origin',(61.5242968087098,0.,0.));
#5616=CARTESIAN_POINT('Origin',(58.5152881956451,0.,0.));
#5617=CARTESIAN_POINT('Origin',(65.0333054217745,0.,11.6461191435901));
#5618=CARTESIAN_POINT('',(58.1417842183134,-5.99845082347644E-16,10.6461191435901));
#5619=CARTESIAN_POINT('Ctrl Pts',(58.5152881956451,-0.761781030806632,10.9982845496518));
#5620=CARTESIAN_POINT('Ctrl Pts',(58.4654152249681,-0.721092606887457,10.9504395135808));
#5621=CARTESIAN_POINT('Ctrl Pts',(58.4186772780868,-0.675440849291838,10.9059348433374));
#5622=CARTESIAN_POINT('Ctrl Pts',(58.3120945049187,-0.549535986315256,10.8049911463411));
#5623=CARTESIAN_POINT('Ctrl Pts',(58.2507030237862,-0.453536381338077,10.7474642978206));
#5624=CARTESIAN_POINT('Ctrl Pts',(58.1653214105115,-0.237277778231237,10.6678680788412));
#5625=CARTESIAN_POINT('Ctrl Pts',(58.1417842183134,-0.11672247158404,10.6461191435901));
#5626=CARTESIAN_POINT('Ctrl Pts',(58.1417842183134,-6.93889390390723E-17,
10.6461191435901));
#5627=CARTESIAN_POINT('Ctrl Pts',(58.1417842183134,1.38777878078145E-16,
10.6461191435901));
#5628=CARTESIAN_POINT('Ctrl Pts',(58.1417842183134,0.11672247158404,10.6461191435901));
#5629=CARTESIAN_POINT('Ctrl Pts',(58.1653214105115,0.237277778231238,10.6678680788412));
#5630=CARTESIAN_POINT('Ctrl Pts',(58.2507030237862,0.453536381338078,10.7474642978206));
#5631=CARTESIAN_POINT('Ctrl Pts',(58.3120945049187,0.549535986315257,10.8049911463411));
#5632=CARTESIAN_POINT('Ctrl Pts',(58.4186772780868,0.675440849291838,10.9059348433374));
#5633=CARTESIAN_POINT('Ctrl Pts',(58.4654152249681,0.721092606887457,10.9504395135808));
#5634=CARTESIAN_POINT('Ctrl Pts',(58.5152881956451,0.761781030806632,10.9982845496518));
#5635=CARTESIAN_POINT('Origin',(58.259303580337,0.,0.));
#5636=CARTESIAN_POINT('Origin',(58.5152881956451,0.,0.));
#5637=CARTESIAN_POINT('',(58.259303580337,-1.31835865745385E-15,10.765215394118));
#5638=CARTESIAN_POINT('Origin',(61.5242968087098,0.,0.));
#5639=CARTESIAN_POINT('Origin',(65.0333054217745,0.,0.));
#5640=CARTESIAN_POINT('Origin',(57.9998593353039,0.,-9.50579594738959));
#5641=CARTESIAN_POINT('',(57.9998593353039,-1.16412425803185E-15,9.50579594738959));
#5642=CARTESIAN_POINT('Origin',(57.9998593353039,0.,0.));
#5643=CARTESIAN_POINT('Origin',(54.0059764245311,0.,0.));
#5644=CARTESIAN_POINT('',(54.0059764245311,-1.16412425803185E-15,9.50579594738959));
#5645=CARTESIAN_POINT('',(0.,0.,0.));
#5646=CARTESIAN_POINT('Origin',(4.25,0.,0.));
#5647=CARTESIAN_POINT('',(4.,1.,6.1419892173341));
#5648=CARTESIAN_POINT('',(4.5,1.,5.63481747112189));
#5649=CARTESIAN_POINT('Ctrl Pts',(4.,1.,6.1419892173341));
#5650=CARTESIAN_POINT('Ctrl Pts',(4.26076632571102,1.,5.87778926153153));
#5651=CARTESIAN_POINT('Ctrl Pts',(4.5,1.,5.63481747112189));
#5652=CARTESIAN_POINT('',(4.5,-1.,5.63481747112189));
#5653=CARTESIAN_POINT('Origin',(4.5,0.,0.));
#5654=CARTESIAN_POINT('',(4.,-1.,6.1419892173341));
#5655=CARTESIAN_POINT('Ctrl Pts',(4.5,-1.,5.63481747112189));
#5656=CARTESIAN_POINT('Ctrl Pts',(4.26076632570315,-1.,5.87778926153949));
#5657=CARTESIAN_POINT('Ctrl Pts',(4.,-1.,6.1419892173341));
#5658=CARTESIAN_POINT('Origin',(4.,0.,0.));
#5659=CARTESIAN_POINT('Origin',(4.5,0.,-0.0373945338826487));
#5660=CARTESIAN_POINT('',(4.5,1.,4.6157817005232));
#5661=CARTESIAN_POINT('',(4.5,1.,9.13904432441494));
#5662=CARTESIAN_POINT('',(4.5,-1.,4.61578170052319));
#5663=CARTESIAN_POINT('Origin',(4.5,0.,0.));
#5664=CARTESIAN_POINT('',(4.5,-1.,-9.13904432441494));
#5665=CARTESIAN_POINT('Origin',(1.5,1.,6.64807454522257));
#5666=CARTESIAN_POINT('',(2.,1.,6.1419892173341));
#5667=CARTESIAN_POINT('',(1.5,1.,6.1419892173341));
#5668=CARTESIAN_POINT('',(1.5,1.,5.63481747112189));
#5669=CARTESIAN_POINT('Ctrl Pts',(1.5,1.,5.63481747112189));
#5670=CARTESIAN_POINT('Ctrl Pts',(1.73923367429685,1.,5.87778926153949));
#5671=CARTESIAN_POINT('Ctrl Pts',(2.,1.,6.1419892173341));
#5672=CARTESIAN_POINT('',(1.5,1.,4.6157817005232));
#5673=CARTESIAN_POINT('',(1.5,1.,9.13904432441494));
#5674=CARTESIAN_POINT('',(1.5,1.,4.6157817005232));
#5675=CARTESIAN_POINT('Origin',(1.75,0.,0.));
#5676=CARTESIAN_POINT('',(2.,-1.,6.1419892173341));
#5677=CARTESIAN_POINT('',(1.5,-1.,5.63481747112189));
#5678=CARTESIAN_POINT('Ctrl Pts',(2.,-1.,6.1419892173341));
#5679=CARTESIAN_POINT('Ctrl Pts',(1.73923367428898,-1.,5.87778926153153));
#5680=CARTESIAN_POINT('Ctrl Pts',(1.5,-1.,5.63481747112189));
#5681=CARTESIAN_POINT('Origin',(1.5,0.,0.));
#5682=CARTESIAN_POINT('Origin',(2.,0.,0.));
#5683=CARTESIAN_POINT('Origin',(1.5,0.,0.));
#5684=CARTESIAN_POINT('',(1.5,-1.,6.1419892173341));
#5685=CARTESIAN_POINT('Origin',(1.5,-1.,4.61578170052319));
#5686=CARTESIAN_POINT('',(1.5,-1.,4.61578170052319));
#5687=CARTESIAN_POINT('',(1.5,-1.,4.61578170052319));
#5688=CARTESIAN_POINT('',(1.5,-1.,-9.13904432441494));
#5689=CARTESIAN_POINT('Origin',(1.5,0.,0.));
#5690=CARTESIAN_POINT('Origin',(1.5,0.,0.));
#5691=CARTESIAN_POINT('Origin',(1.5,0.,-0.0373945338826487));
#5692=CARTESIAN_POINT('',(0.,0.,0.));
#5693=CARTESIAN_POINT('Origin',(10.9788681304862,1.34514335437282,16.));
#5694=CARTESIAN_POINT('',(11.0183695787139,0.846706161149926,15.5));
#5695=CARTESIAN_POINT('',(11.0183695787139,0.846706161149926,12.));
#5696=CARTESIAN_POINT('',(11.0183695787139,0.846706161149926,16.));
#5697=CARTESIAN_POINT('',(11.4651166898695,1.46160080796717,15.5));
#5698=CARTESIAN_POINT('Ctrl Pts',(11.4651166898695,1.46160080796717,15.5));
#5699=CARTESIAN_POINT('Ctrl Pts',(11.4651166898695,1.46160080796717,15.5327258400527));
#5700=CARTESIAN_POINT('Ctrl Pts',(11.4660168040712,1.45801754115624,15.5654293765226));
#5701=CARTESIAN_POINT('Ctrl Pts',(11.4691283383932,1.44362639892173,15.6290406866894));
#5702=CARTESIAN_POINT('Ctrl Pts',(11.4713273005329,1.43286974240523,15.6598442001575));
#5703=CARTESIAN_POINT('Ctrl Pts',(11.4765149298,1.39787805797502,15.7305775282065));
#5704=CARTESIAN_POINT('Ctrl Pts',(11.4793990336829,1.37028664210651,15.7678051908843));
#5705=CARTESIAN_POINT('Ctrl Pts',(11.4782015086689,1.30346706538635,15.8295297239576));
#5706=CARTESIAN_POINT('Ctrl Pts',(11.4743049792552,1.26629507509822,15.853094168515));
#5707=CARTESIAN_POINT('Ctrl Pts',(11.4549023017239,1.18683333243691,15.8881049113845));
#5708=CARTESIAN_POINT('Ctrl Pts',(11.4397065054753,1.14620200545152,15.8989286877205));
#5709=CARTESIAN_POINT('Ctrl Pts',(11.396404023885,1.06610334829151,15.9101071881998));
#5710=CARTESIAN_POINT('Ctrl Pts',(11.3678139645159,1.02747859678379,15.909753701168));
#5711=CARTESIAN_POINT('Ctrl Pts',(11.302566216258,0.961281878811867,15.8967861544805));
#5712=CARTESIAN_POINT('Ctrl Pts',(11.2665927725368,0.934059884456842,15.8843843767206));
#5713=CARTESIAN_POINT('Ctrl Pts',(11.1952176199532,0.89256475492642,15.8454873880819));
#5714=CARTESIAN_POINT('Ctrl Pts',(11.1614633805605,0.878606603360417,15.8203384131985));
#5715=CARTESIAN_POINT('Ctrl Pts',(11.0976617200424,0.858171109417801,15.7531662441803));
#5716=CARTESIAN_POINT('Ctrl Pts',(11.0703452620001,0.85319590461791,15.7112656542922));
#5717=CARTESIAN_POINT('Ctrl Pts',(11.0294097048913,0.84722400890498,15.6129130718351));
#5718=CARTESIAN_POINT('Ctrl Pts',(11.0183695787139,0.846706161149926,15.5565891907874));
#5719=CARTESIAN_POINT('Ctrl Pts',(11.0183695787139,0.846706161149926,15.5));
#5720=CARTESIAN_POINT('',(11.4651166898695,1.46160080796717,12.));
#5721=CARTESIAN_POINT('',(11.4651166898695,1.46160080796717,16.));
#5722=CARTESIAN_POINT('Origin',(10.9788681304862,1.34514335437282,12.));
#5723=CARTESIAN_POINT('Origin',(12.1231154122328,2.17648766711626,16.));
#5724=CARTESIAN_POINT('',(11.862098723781,1.75002513845795,15.5));
#5725=CARTESIAN_POINT('',(11.862098723781,1.75002513845795,12.));
#5726=CARTESIAN_POINT('',(11.862098723781,1.75002513845795,16.));
#5727=CARTESIAN_POINT('',(12.5849507340066,1.98489399404177,15.5));
#5728=CARTESIAN_POINT('Ctrl Pts',(12.5849507340066,1.98489399404177,15.5));
#5729=CARTESIAN_POINT('Ctrl Pts',(12.5849507340066,1.98489399404177,15.5315974346976));
#5730=CARTESIAN_POINT('Ctrl Pts',(12.5836637760388,1.98169929993151,15.5631757175052));
#5731=CARTESIAN_POINT('Ctrl Pts',(12.5781379778504,1.96911950577423,15.6247606509986));
#5732=CARTESIAN_POINT('Ctrl Pts',(12.5739120210771,1.9597668107847,15.6546762688613));
#5733=CARTESIAN_POINT('Ctrl Pts',(12.5584805763086,1.92978725799424,15.7249493973573));
#5734=CARTESIAN_POINT('Ctrl Pts',(12.5451313949437,1.906259901776,15.762620760625));
#5735=CARTESIAN_POINT('Ctrl Pts',(12.5060588179609,1.85338430197355,15.8255830998499));
#5736=CARTESIAN_POINT('Ctrl Pts',(12.4815883321467,1.82554632233921,15.8498680529139));
#5737=CARTESIAN_POINT('Ctrl Pts',(12.4192606585594,1.77146870244053,15.8866893895236));
#5738=CARTESIAN_POINT('Ctrl Pts',(12.382396883207,1.74656759203559,15.8982106592639));
#5739=CARTESIAN_POINT('Ctrl Pts',(12.2978763951411,1.70550952857365,15.9102329913456));
#5740=CARTESIAN_POINT('Ctrl Pts',(12.2502943035319,1.69050766300347,15.909874133055));
#5741=CARTESIAN_POINT('Ctrl Pts',(12.1579952361435,1.67568037378513,15.8963684971709));
#5742=CARTESIAN_POINT('Ctrl Pts',(12.1140332395114,1.67487990467903,15.8841705706778));
#5743=CARTESIAN_POINT('Ctrl Pts',(12.032581997837,1.68306934122621,15.8458060158298));
#5744=CARTESIAN_POINT('Ctrl Pts',(11.9968182859843,1.69165869793162,15.8205491017219));
#5745=CARTESIAN_POINT('Ctrl Pts',(11.9330125310872,1.71268387513612,15.7531986669259));
#5746=CARTESIAN_POINT('Ctrl Pts',(11.9079924325872,1.7247105935723,15.7113185385228));
#5747=CARTESIAN_POINT('Ctrl Pts',(11.8713435677214,1.74394867728652,15.6129675013504));
#5748=CARTESIAN_POINT('Ctrl Pts',(11.862098723781,1.75002513845795,15.5566167040035));
#5749=CARTESIAN_POINT('Ctrl Pts',(11.862098723781,1.75002513845795,15.5));
#5750=CARTESIAN_POINT('',(12.5849507340066,1.98489399404177,12.));
#5751=CARTESIAN_POINT('',(12.5849507340066,1.98489399404177,16.));
#5752=CARTESIAN_POINT('Origin',(12.1231154122328,2.17648766711626,12.));
#5753=CARTESIAN_POINT('Origin',(13.537482835541,2.17648766711626,16.));
#5754=CARTESIAN_POINT('',(13.0756475137673,1.98489399404177,15.5));
#5755=CARTESIAN_POINT('',(13.0756475137673,1.98489399404177,12.));
#5756=CARTESIAN_POINT('',(13.0756475137673,1.98489399404177,16.));
#5757=CARTESIAN_POINT('',(13.7984995239928,1.75002513845795,15.5));
#5758=CARTESIAN_POINT('Ctrl Pts',(13.7984995239928,1.75002513845795,15.5));
#5759=CARTESIAN_POINT('Ctrl Pts',(13.7984995239928,1.75002513845795,15.5315974346976));
#5760=CARTESIAN_POINT('Ctrl Pts',(13.7955805590423,1.74819703154467,15.5631757175052));
#5761=CARTESIAN_POINT('Ctrl Pts',(13.7837158769179,1.74126774696798,15.6247606509986));
#5762=CARTESIAN_POINT('Ctrl Pts',(13.7747996298867,1.73618521284642,15.6546762688613));
#5763=CARTESIAN_POINT('Ctrl Pts',(13.7446937898207,1.72100162081168,15.7249493973573));
#5764=CARTESIAN_POINT('Ctrl Pts',(13.7200650422249,1.70981404173489,15.762620760625));
#5765=CARTESIAN_POINT('Ctrl Pts',(13.6573751656619,1.69000306742646,15.8255830998499));
#5766=CARTESIAN_POINT('Ctrl Pts',(13.6212153728949,1.68186505949125,15.8498680529139));
#5767=CARTESIAN_POINT('Ctrl Pts',(13.5390051982874,1.67475063332216,15.8866893895236));
#5768=CARTESIAN_POINT('Ctrl Pts',(13.4945452720888,1.67627319532172,15.8982106592639));
#5769=CARTESIAN_POINT('Ctrl Pts',(13.40203343668,1.69273642062657,15.9102329913456));
#5770=CARTESIAN_POINT('Ctrl Pts',(13.3547208406011,1.70856770815414,15.909874133055));
#5771=CARTESIAN_POINT('Ctrl Pts',(13.271334064585,1.7508242098072,15.8963684971709));
#5772=CARTESIAN_POINT('Ctrl Pts',(13.2352975582675,1.77601682997859,15.8841705706778));
#5773=CARTESIAN_POINT('Ctrl Pts',(13.174215749567,1.83051806195672,15.8458060158298));
#5774=CARTESIAN_POINT('Ctrl Pts',(13.1503309960943,1.85848837989641,15.8205491017219));
#5775=CARTESIAN_POINT('Ctrl Pts',(13.1110693451313,1.91300218730451,15.7531986669259));
#5776=CARTESIAN_POINT('Ctrl Pts',(13.0978967879741,1.93743845181515,15.7113185385228));
#5777=CARTESIAN_POINT('Ctrl Pts',(13.0795550953627,1.97454405076051,15.6129675013504));
#5778=CARTESIAN_POINT('Ctrl Pts',(13.0756475137673,1.98489399404177,15.5566167040035));
#5779=CARTESIAN_POINT('Ctrl Pts',(13.0756475137673,1.98489399404177,15.5));
#5780=CARTESIAN_POINT('',(13.7984995239928,1.75002513845795,12.));
#5781=CARTESIAN_POINT('',(13.7984995239928,1.75002513845795,16.));
#5782=CARTESIAN_POINT('Origin',(13.537482835541,2.17648766711626,12.));
#5783=CARTESIAN_POINT('Origin',(14.6817301172876,1.34514335437282,16.));
#5784=CARTESIAN_POINT('',(14.1954815579043,1.46160080796717,15.5));
#5785=CARTESIAN_POINT('',(14.1954815579043,1.46160080796717,12.));
#5786=CARTESIAN_POINT('',(14.1954815579043,1.46160080796717,16.));
#5787=CARTESIAN_POINT('',(14.6422286690599,0.846706161149931,15.5));
#5788=CARTESIAN_POINT('Ctrl Pts',(14.6422286690599,0.84670616114993,15.5));
#5789=CARTESIAN_POINT('Ctrl Pts',(14.6422286690599,0.84670616114993,15.5328840768056));
#5790=CARTESIAN_POINT('Ctrl Pts',(14.6385068660889,0.846959432552971,15.5657453762427));
#5791=CARTESIAN_POINT('Ctrl Pts',(14.6237151505491,0.848465062627269,15.6296563210017));
#5792=CARTESIAN_POINT('Ctrl Pts',(14.6126966763369,0.849713657088164,15.660598638283));
#5793=CARTESIAN_POINT('Ctrl Pts',(14.5776079356378,0.855659177572526,15.7313318911412));
#5794=CARTESIAN_POINT('Ctrl Pts',(14.550441321518,0.861482780240192,15.7684373555081));
#5795=CARTESIAN_POINT('Ctrl Pts',(14.4872412940069,0.883356517365064,15.8299542128302));
#5796=CARTESIAN_POINT('Ctrl Pts',(14.4530989465518,0.898598843657317,15.8534299122416));
#5797=CARTESIAN_POINT('Ctrl Pts',(14.3835813171714,0.941686180099718,15.8882855843752));
#5798=CARTESIAN_POINT('Ctrl Pts',(14.3496795039836,0.968726370854913,15.89904798654));
#5799=CARTESIAN_POINT('Ctrl Pts',(14.2869736205215,1.03471311698917,15.9101249054252));
#5800=CARTESIAN_POINT('Ctrl Pts',(14.2591225164167,1.07386600486173,15.9097261007587));
#5801=CARTESIAN_POINT('Ctrl Pts',(14.2165374803957,1.15619086111778,15.8966960156851));
#5802=CARTESIAN_POINT('Ctrl Pts',(14.201856352804,1.19858800968841,15.8843371675477));
#5803=CARTESIAN_POINT('Ctrl Pts',(14.1844547128968,1.27913917972905,15.8455544418483));
#5804=CARTESIAN_POINT('Ctrl Pts',(14.1816023263936,1.31560737922412,15.8203829360199));
#5805=CARTESIAN_POINT('Ctrl Pts',(14.1818824447642,1.38264039078621,15.7531735756887));
#5806=CARTESIAN_POINT('Ctrl Pts',(14.1855913480644,1.41015640885706,15.7112772176026));
#5807=CARTESIAN_POINT('Ctrl Pts',(14.1925617954654,1.4509387910301,15.6129247586851));
#5808=CARTESIAN_POINT('Ctrl Pts',(14.1954815579043,1.46160080796717,15.5565950982509));
#5809=CARTESIAN_POINT('Ctrl Pts',(14.1954815579043,1.46160080796717,15.5));
#5810=CARTESIAN_POINT('',(14.6422286690599,0.846706161149931,12.));
#5811=CARTESIAN_POINT('',(14.6422286690599,0.84670616114993,16.));
#5812=CARTESIAN_POINT('Origin',(14.6817301172876,1.34514335437282,12.));
#5813=CARTESIAN_POINT('Origin',(15.1187936873802,2.22044604925031E-15,16.));
#5814=CARTESIAN_POINT('',(14.793862313091,0.380025791233419,15.5));
#5815=CARTESIAN_POINT('',(14.793862313091,0.380025791233419,12.));
#5816=CARTESIAN_POINT('',(14.793862313091,0.380025791233419,16.));
#5817=CARTESIAN_POINT('',(14.793862313091,-0.380025791233415,15.5));
#5818=CARTESIAN_POINT('Ctrl Pts',(14.793862313091,-0.380025791233415,15.5));
#5819=CARTESIAN_POINT('Ctrl Pts',(14.793862313091,-0.380025791233415,15.5301189378802));
#5820=CARTESIAN_POINT('Ctrl Pts',(14.7914649109341,-0.378014471067455,15.5602222957306));
#5821=CARTESIAN_POINT('Ctrl Pts',(14.7820629540924,-0.369665255070382,15.619473583796));
#5822=CARTESIAN_POINT('Ctrl Pts',(14.7750166556806,-0.363286881363678,15.6485271997616));
#5823=CARTESIAN_POINT('Ctrl Pts',(14.7530701481314,-0.341440768177844,15.7162986234851));
#5824=CARTESIAN_POINT('Ctrl Pts',(14.736260482547,-0.323422662348315,15.7528086416089));
#5825=CARTESIAN_POINT('Ctrl Pts',(14.6988036079793,-0.273200108532066,15.8176504259456));
#5826=CARTESIAN_POINT('Ctrl Pts',(14.6789741278953,-0.241442615310855,15.8439766371743));
#5827=CARTESIAN_POINT('Ctrl Pts',(14.649052119539,-0.174242241359358,15.8790044118403));
#5828=CARTESIAN_POINT('Ctrl Pts',(14.6382480050478,-0.142377760727725,15.8899019417197));
#5829=CARTESIAN_POINT('Ctrl Pts',(14.6253569192039,-0.0844582380039889,
15.9024084088928));
#5830=CARTESIAN_POINT('Ctrl Pts',(14.62170907487,-0.0595388860092602,15.9057258119584));
#5831=CARTESIAN_POINT('Ctrl Pts',(14.6184132964927,-0.0116648059065203,
15.9087259343201));
#5832=CARTESIAN_POINT('Ctrl Pts',(14.6184025825216,0.0111982465765552,15.9087354208236));
#5833=CARTESIAN_POINT('Ctrl Pts',(14.6216515805607,0.0590421319272091,15.9057784384354));
#5834=CARTESIAN_POINT('Ctrl Pts',(14.6252687876419,0.08393313812265,15.9024901407371));
#5835=CARTESIAN_POINT('Ctrl Pts',(14.6380668952534,0.141740583709937,15.8900828025045));
#5836=CARTESIAN_POINT('Ctrl Pts',(14.6487962756114,0.173538618517613,15.8792727935245));
#5837=CARTESIAN_POINT('Ctrl Pts',(14.6782561696043,0.239992102668341,15.8448561504018));
#5838=CARTESIAN_POINT('Ctrl Pts',(14.6976208691953,0.271333339752337,15.8192728778931));
#5839=CARTESIAN_POINT('Ctrl Pts',(14.7371948204043,0.324961457403922,15.7516236294289));
#5840=CARTESIAN_POINT('Ctrl Pts',(14.7561115708548,0.34471876336765,15.709950843486));
#5841=CARTESIAN_POINT('Ctrl Pts',(14.785345858337,0.373200978981364,15.6122094926721));
#5842=CARTESIAN_POINT('Ctrl Pts',(14.793862313091,0.380025791233419,15.556233591069));
#5843=CARTESIAN_POINT('Ctrl Pts',(14.793862313091,0.380025791233419,15.5));
#5844=CARTESIAN_POINT('',(14.793862313091,-0.380025791233415,12.));
#5845=CARTESIAN_POINT('',(14.793862313091,-0.380025791233415,16.));
#5846=CARTESIAN_POINT('Origin',(15.1187936873802,2.22044604925031E-15,12.));
#5847=CARTESIAN_POINT('Origin',(14.6817301172876,-1.34514335437282,16.));
#5848=CARTESIAN_POINT('',(14.6422286690599,-0.846706161149925,15.5));
#5849=CARTESIAN_POINT('',(14.6422286690599,-0.846706161149925,12.));
#5850=CARTESIAN_POINT('',(14.6422286690599,-0.846706161149924,16.));
#5851=CARTESIAN_POINT('',(14.1954815579043,-1.46160080796717,15.5));
#5852=CARTESIAN_POINT('Ctrl Pts',(14.1954815579043,-1.46160080796717,15.5));
#5853=CARTESIAN_POINT('Ctrl Pts',(14.1954815579043,-1.46160080796717,15.5328840768056));
#5854=CARTESIAN_POINT('Ctrl Pts',(14.1945723329548,-1.45798289783153,15.5657453762427));
#5855=CARTESIAN_POINT('Ctrl Pts',(14.1914333807704,-1.44344987510003,15.6296563210017));
#5856=CARTESIAN_POINT('Ctrl Pts',(14.1892159688849,-1.43258484649331,15.660598638283));
#5857=CARTESIAN_POINT('Ctrl Pts',(14.1840274776971,-1.39737620413281,15.7313318911412));
#5858=CARTESIAN_POINT('Ctrl Pts',(14.1811711075199,-1.36973962655568,15.7684373555081));
#5859=CARTESIAN_POINT('Ctrl Pts',(14.1824443852023,-1.30287347205919,15.8299542128302));
#5860=CARTESIAN_POINT('Ctrl Pts',(14.1863901333546,-1.26569203217221,15.8534299122416));
#5861=CARTESIAN_POINT('Ctrl Pts',(14.2058864965607,-1.18626211854957,15.8882855843752));
#5862=CARTESIAN_POINT('Ctrl Pts',(14.2211270097652,-1.14566369972857,15.89904798654));
#5863=CARTESIAN_POINT('Ctrl Pts',(14.2645069510282,-1.06563583469299,15.9101249054252));
#5864=CARTESIAN_POINT('Ctrl Pts',(14.2931370956907,-1.0270489529166,15.9097261007587));
#5865=CARTESIAN_POINT('Ctrl Pts',(14.3582731868495,-0.961108397269499,15.8966960156851));
#5866=CARTESIAN_POINT('Ctrl Pts',(14.3940585533475,-0.93404437578549,15.8843371675477));
#5867=CARTESIAN_POINT('Ctrl Pts',(14.4652898660485,-0.892602752298236,15.8455544418483));
#5868=CARTESIAN_POINT('Ctrl Pts',(14.4990917489119,-0.878620678129173,15.8203829360199));
#5869=CARTESIAN_POINT('Ctrl Pts',(14.5629304927018,-0.858172746774003,15.7531735756887));
#5870=CARTESIAN_POINT('Ctrl Pts',(14.5902458951409,-0.853197206224569,15.7112772176026));
#5871=CARTESIAN_POINT('Ctrl Pts',(14.6311862321619,-0.847224046484188,15.6129247586851));
#5872=CARTESIAN_POINT('Ctrl Pts',(14.6422286690599,-0.846706161149924,15.5565950982509));
#5873=CARTESIAN_POINT('Ctrl Pts',(14.6422286690599,-0.846706161149924,15.5));
#5874=CARTESIAN_POINT('',(14.1954815579043,-1.46160080796717,12.));
#5875=CARTESIAN_POINT('',(14.1954815579043,-1.46160080796717,16.));
#5876=CARTESIAN_POINT('Origin',(14.6817301172876,-1.34514335437282,12.));
#5877=CARTESIAN_POINT('Origin',(13.537482835541,-2.17648766711626,16.));
#5878=CARTESIAN_POINT('',(13.7984995239928,-1.75002513845795,15.5));
#5879=CARTESIAN_POINT('',(13.7984995239928,-1.75002513845795,12.));
#5880=CARTESIAN_POINT('',(13.7984995239928,-1.75002513845795,16.));
#5881=CARTESIAN_POINT('',(13.0756475137673,-1.98489399404177,15.5));
#5882=CARTESIAN_POINT('Ctrl Pts',(13.0756475137673,-1.98489399404178,15.5));
#5883=CARTESIAN_POINT('Ctrl Pts',(13.0756475137673,-1.98489399404178,15.5315974346976));
#5884=CARTESIAN_POINT('Ctrl Pts',(13.076934471735,-1.98169929993151,15.5631757175052));
#5885=CARTESIAN_POINT('Ctrl Pts',(13.0824602699234,-1.96911950577423,15.6247606509986));
#5886=CARTESIAN_POINT('Ctrl Pts',(13.0866862266967,-1.9597668107847,15.6546762688613));
#5887=CARTESIAN_POINT('Ctrl Pts',(13.1021176714653,-1.92978725799424,15.7249493973573));
#5888=CARTESIAN_POINT('Ctrl Pts',(13.1154668528302,-1.906259901776,15.762620760625));
#5889=CARTESIAN_POINT('Ctrl Pts',(13.1545394298129,-1.85338430197355,15.8255830998499));
#5890=CARTESIAN_POINT('Ctrl Pts',(13.1790099156272,-1.82554632233921,15.8498680529139));
#5891=CARTESIAN_POINT('Ctrl Pts',(13.2413375892144,-1.77146870244053,15.8866893895236));
#5892=CARTESIAN_POINT('Ctrl Pts',(13.2782013645668,-1.74656759203558,15.8982106592639));
#5893=CARTESIAN_POINT('Ctrl Pts',(13.3627218526327,-1.70550952857365,15.9102329913456));
#5894=CARTESIAN_POINT('Ctrl Pts',(13.410303944242,-1.69050766300347,15.909874133055));
#5895=CARTESIAN_POINT('Ctrl Pts',(13.5026030116303,-1.67568037378513,15.8963684971709));
#5896=CARTESIAN_POINT('Ctrl Pts',(13.5465650082624,-1.67487990467903,15.8841705706778));
#5897=CARTESIAN_POINT('Ctrl Pts',(13.6280162499368,-1.68306934122621,15.8458060158298));
#5898=CARTESIAN_POINT('Ctrl Pts',(13.6637799617895,-1.69165869793162,15.8205491017219));
#5899=CARTESIAN_POINT('Ctrl Pts',(13.7275857166867,-1.71268387513612,15.7531986669259));
#5900=CARTESIAN_POINT('Ctrl Pts',(13.7526058151867,-1.7247105935723,15.7113185385228));
#5901=CARTESIAN_POINT('Ctrl Pts',(13.7892546800524,-1.74394867728652,15.6129675013504));
#5902=CARTESIAN_POINT('Ctrl Pts',(13.7984995239928,-1.75002513845795,15.5566167040035));
#5903=CARTESIAN_POINT('Ctrl Pts',(13.7984995239928,-1.75002513845795,15.5));
#5904=CARTESIAN_POINT('',(13.0756475137673,-1.98489399404177,12.));
#5905=CARTESIAN_POINT('',(13.0756475137673,-1.98489399404177,16.));
#5906=CARTESIAN_POINT('Origin',(13.537482835541,-2.17648766711626,12.));
#5907=CARTESIAN_POINT('Origin',(12.1231154122328,-2.17648766711627,16.));
#5908=CARTESIAN_POINT('',(12.5849507340066,-1.98489399404177,15.5));
#5909=CARTESIAN_POINT('',(12.5849507340066,-1.98489399404177,12.));
#5910=CARTESIAN_POINT('',(12.5849507340066,-1.98489399404177,16.));
#5911=CARTESIAN_POINT('',(11.862098723781,-1.75002513845795,15.5));
#5912=CARTESIAN_POINT('Ctrl Pts',(11.862098723781,-1.75002513845795,15.5));
#5913=CARTESIAN_POINT('Ctrl Pts',(11.862098723781,-1.75002513845795,15.5315974346976));
#5914=CARTESIAN_POINT('Ctrl Pts',(11.8650176887316,-1.74819703154467,15.5631757175052));
#5915=CARTESIAN_POINT('Ctrl Pts',(11.876882370856,-1.74126774696798,15.6247606509986));
#5916=CARTESIAN_POINT('Ctrl Pts',(11.8857986178871,-1.73618521284643,15.6546762688613));
#5917=CARTESIAN_POINT('Ctrl Pts',(11.9159044579532,-1.72100162081169,15.7249493973573));
#5918=CARTESIAN_POINT('Ctrl Pts',(11.9405332055489,-1.7098140417349,15.762620760625));
#5919=CARTESIAN_POINT('Ctrl Pts',(12.003223082112,-1.69000306742646,15.8255830998499));
#5920=CARTESIAN_POINT('Ctrl Pts',(12.039382874879,-1.68186505949125,15.8498680529139));
#5921=CARTESIAN_POINT('Ctrl Pts',(12.1215930494864,-1.67475063332217,15.8866893895236));
#5922=CARTESIAN_POINT('Ctrl Pts',(12.1660529756851,-1.67627319532172,15.8982106592639));
#5923=CARTESIAN_POINT('Ctrl Pts',(12.2585648110939,-1.69273642062657,15.9102329913456));
#5924=CARTESIAN_POINT('Ctrl Pts',(12.3058774071727,-1.70856770815414,15.909874133055));
#5925=CARTESIAN_POINT('Ctrl Pts',(12.3892641831888,-1.75082420980719,15.8963684971709));
#5926=CARTESIAN_POINT('Ctrl Pts',(12.4253006895064,-1.77601682997858,15.8841705706778));
#5927=CARTESIAN_POINT('Ctrl Pts',(12.4863824982069,-1.83051806195672,15.8458060158298));
#5928=CARTESIAN_POINT('Ctrl Pts',(12.5102672516795,-1.85848837989641,15.8205491017219));
#5929=CARTESIAN_POINT('Ctrl Pts',(12.5495289026426,-1.9130021873045,15.7531986669259));
#5930=CARTESIAN_POINT('Ctrl Pts',(12.5627014597997,-1.93743845181514,15.7113185385228));
#5931=CARTESIAN_POINT('Ctrl Pts',(12.5810431524111,-1.97454405076052,15.6129675013504));
#5932=CARTESIAN_POINT('Ctrl Pts',(12.5849507340066,-1.98489399404177,15.5566167040035));
#5933=CARTESIAN_POINT('Ctrl Pts',(12.5849507340066,-1.98489399404177,15.5));
#5934=CARTESIAN_POINT('',(11.862098723781,-1.75002513845795,12.));
#5935=CARTESIAN_POINT('',(11.862098723781,-1.75002513845795,16.));
#5936=CARTESIAN_POINT('Origin',(12.1231154122328,-2.17648766711627,12.));
#5937=CARTESIAN_POINT('Origin',(10.9788681304862,-1.34514335437282,16.));
#5938=CARTESIAN_POINT('',(11.4651166898695,-1.46160080796717,15.5));
#5939=CARTESIAN_POINT('',(11.4651166898695,-1.46160080796717,12.));
#5940=CARTESIAN_POINT('',(11.4651166898695,-1.46160080796717,16.));
#5941=CARTESIAN_POINT('',(11.0183695787139,-0.846706161149927,15.5));
#5942=CARTESIAN_POINT('Ctrl Pts',(11.0183695787139,-0.846706161149927,15.5));
#5943=CARTESIAN_POINT('Ctrl Pts',(11.0183695787139,-0.846706161149927,15.5327258400527));
#5944=CARTESIAN_POINT('Ctrl Pts',(11.0220556185493,-0.84695739201299,15.5654293765226));
#5945=CARTESIAN_POINT('Ctrl Pts',(11.0367039251324,-0.848445254539305,15.6290406866894));
#5946=CARTESIAN_POINT('Ctrl Pts',(11.0476136300772,-0.849677906933497,15.6598442001574));
#5947=CARTESIAN_POINT('Ctrl Pts',(11.0824957651747,-0.855557203465595,15.7305775282065));
#5948=CARTESIAN_POINT('Ctrl Pts',(11.1096279981436,-0.861340474076375,15.7678051908843));
#5949=CARTESIAN_POINT('Ctrl Pts',(11.1728071364189,-0.883127772807806,15.8295297239576));
#5950=CARTESIAN_POINT('Ctrl Pts',(11.2069557061982,-0.898320369211427,15.853094168515));
#5951=CARTESIAN_POINT('Ctrl Pts',(11.2765325572588,-0.941328440996174,15.8881049113845));
#5952=CARTESIAN_POINT('Ctrl Pts',(11.3104794862702,-0.968336272581112,15.8989286877205));
#5953=CARTESIAN_POINT('Ctrl Pts',(11.3732766333986,-1.0342712261584,15.9101071881998));
#5954=CARTESIAN_POINT('Ctrl Pts',(11.4011761407951,-1.07339769304206,15.909753701168));
#5955=CARTESIAN_POINT('Ctrl Pts',(11.4439702977233,-1.15590790002146,15.8967861544805));
#5956=CARTESIAN_POINT('Ctrl Pts',(11.4587435473851,-1.19853273696263,15.8843843767206));
#5957=CARTESIAN_POINT('Ctrl Pts',(11.4761516255951,-1.27923724113745,15.8454873880819));
#5958=CARTESIAN_POINT('Ctrl Pts',(11.4789959829928,-1.3156527365084,15.8203384131985));
#5959=CARTESIAN_POINT('Ctrl Pts',(11.4787154953012,-1.3826466364114,15.7531662441803));
#5960=CARTESIAN_POINT('Ctrl Pts',(11.4750059464849,-1.41016355466825,15.7112656542922));
#5961=CARTESIAN_POINT('Ctrl Pts',(11.4680357739965,-1.4509410002687,15.6129130718351));
#5962=CARTESIAN_POINT('Ctrl Pts',(11.4651166898695,-1.46160080796717,15.5565891907874));
#5963=CARTESIAN_POINT('Ctrl Pts',(11.4651166898695,-1.46160080796717,15.5));
#5964=CARTESIAN_POINT('',(11.0183695787139,-0.846706161149927,12.));
#5965=CARTESIAN_POINT('',(11.0183695787139,-0.846706161149927,16.));
#5966=CARTESIAN_POINT('Origin',(10.9788681304862,-1.34514335437282,12.));
#5967=CARTESIAN_POINT('Origin',(12.8302991238869,0.,12.));
#5968=CARTESIAN_POINT('Origin',(12.8302991238869,0.,12.));
#5969=CARTESIAN_POINT('Origin',(12.8302991238869,0.,12.));
#5970=CARTESIAN_POINT('Origin',(12.8302991238869,0.,12.));
#5971=CARTESIAN_POINT('Origin',(12.8302991238869,0.,12.));
#5972=CARTESIAN_POINT('Origin',(12.8302991238869,0.,12.));
#5973=CARTESIAN_POINT('Origin',(12.8302991238869,0.,12.));
#5974=CARTESIAN_POINT('Origin',(12.8302991238869,0.,12.));
#5975=CARTESIAN_POINT('Origin',(12.8302991238869,0.,12.));
#5976=CARTESIAN_POINT('',(10.8667359346828,-0.380025791233421,12.));
#5977=CARTESIAN_POINT('Origin',(12.8302991238869,0.,12.));
#5978=CARTESIAN_POINT('',(10.8667359346828,0.380025791233421,12.));
#5979=CARTESIAN_POINT('Origin',(10.5418045603937,0.,12.));
#5980=CARTESIAN_POINT('Origin',(12.8302991238869,0.,12.));
#5981=CARTESIAN_POINT('',(11.8302991238869,-1.22464679914735E-16,12.));
#5982=CARTESIAN_POINT('Origin',(12.8302991238869,0.,12.));
#5983=CARTESIAN_POINT('Origin',(12.8302991238869,0.,12.));
#5984=CARTESIAN_POINT('',(10.8667359346828,-0.38002579123342,15.5));
#5985=CARTESIAN_POINT('Origin',(12.8302991238869,0.,15.5));
#5986=CARTESIAN_POINT('',(10.8667359346828,-0.380025791233421,16.));
#5987=CARTESIAN_POINT('Origin',(12.8302991238869,0.,12.));
#5988=CARTESIAN_POINT('Origin',(12.8302991238869,0.,15.5));
#5989=CARTESIAN_POINT('Origin',(12.8302991238869,0.,12.));
#5990=CARTESIAN_POINT('Origin',(12.8302991238869,0.,15.5));
#5991=CARTESIAN_POINT('Origin',(12.8302991238869,0.,12.));
#5992=CARTESIAN_POINT('Origin',(12.8302991238869,0.,15.5));
#5993=CARTESIAN_POINT('Origin',(12.8302991238869,0.,12.));
#5994=CARTESIAN_POINT('Origin',(12.8302991238869,0.,15.5));
#5995=CARTESIAN_POINT('Origin',(12.8302991238869,0.,12.));
#5996=CARTESIAN_POINT('Origin',(12.8302991238869,0.,15.5));
#5997=CARTESIAN_POINT('Origin',(12.8302991238869,0.,12.));
#5998=CARTESIAN_POINT('Origin',(12.8302991238869,0.,15.5));
#5999=CARTESIAN_POINT('Origin',(12.8302991238869,0.,12.));
#6000=CARTESIAN_POINT('Origin',(12.8302991238869,0.,15.5));
#6001=CARTESIAN_POINT('Origin',(12.8302991238869,0.,12.));
#6002=CARTESIAN_POINT('Origin',(12.8302991238869,0.,15.5));
#6003=CARTESIAN_POINT('Origin',(12.8302991238869,0.,15.5));
#6004=CARTESIAN_POINT('',(11.3302991238869,1.83697019872103E-16,16.));
#6005=CARTESIAN_POINT('Origin',(12.8302991238869,0.,16.));
#6006=CARTESIAN_POINT('',(11.0418045603937,-2.18386077671221E-16,15.9083759136321));
#6007=CARTESIAN_POINT('Origin',(11.3302991238869,-1.83697019872103E-16,
15.5));
#6008=CARTESIAN_POINT('Ctrl Pts',(11.0418045603937,-2.17744741094999E-16,
15.9083759136321));
#6009=CARTESIAN_POINT('Ctrl Pts',(11.0418045603937,-0.0333269392899449,
15.9083759136321));
#6010=CARTESIAN_POINT('Ctrl Pts',(11.0384294338572,-0.0666007585217244,
15.9054111603401));
#6011=CARTESIAN_POINT('Ctrl Pts',(11.0247216398412,-0.134678328230504,15.8922768955596));
#6012=CARTESIAN_POINT('Ctrl Pts',(11.0136953982254,-0.168722451358547,15.8813576283571));
#6013=CARTESIAN_POINT('Ctrl Pts',(10.9836162130091,-0.237730651178781,15.84648748042));
#6014=CARTESIAN_POINT('Ctrl Pts',(10.9641176217848,-0.269612450661452,15.8209662339571));
#6015=CARTESIAN_POINT('Ctrl Pts',(10.9242382544975,-0.324013302894191,15.7533173172479));
#6016=CARTESIAN_POINT('Ctrl Pts',(10.9051561320036,-0.344027884939244,15.7116694990272));
#6017=CARTESIAN_POINT('Ctrl Pts',(10.8754426059288,-0.373057962817857,15.6134141633368));
#6018=CARTESIAN_POINT('Ctrl Pts',(10.8667359346828,-0.380025791233421,15.5568425534222));
#6019=CARTESIAN_POINT('Ctrl Pts',(10.8667359346828,-0.380025791233421,15.5));
#6020=CARTESIAN_POINT('',(10.8667359346828,0.38002579123342,15.5));
#6021=CARTESIAN_POINT('Origin',(12.8302991238869,0.,15.5));
#6022=CARTESIAN_POINT('Ctrl Pts',(10.8667359346828,0.38002579123342,15.5));
#6023=CARTESIAN_POINT('Ctrl Pts',(10.8667359346828,0.38002579123342,15.5287883283061));
#6024=CARTESIAN_POINT('Ctrl Pts',(10.8689246936405,0.378186511904044,15.5575638011946));
#6025=CARTESIAN_POINT('Ctrl Pts',(10.8775010031577,0.370595290430779,15.6141318495287));
#6026=CARTESIAN_POINT('Ctrl Pts',(10.8839020018485,0.364829650654932,15.641855828518));
#6027=CARTESIAN_POINT('Ctrl Pts',(10.9048993108626,0.344216382575075,15.7100185500455));
#6028=CARTESIAN_POINT('Ctrl Pts',(10.9219087613342,0.326315405731202,15.7480224050071));
#6029=CARTESIAN_POINT('Ctrl Pts',(10.9597410970604,0.276288530513651,15.8146310640371));
#6030=CARTESIAN_POINT('Ctrl Pts',(10.9796822362452,0.244921275640039,15.8414816023624));
#6031=CARTESIAN_POINT('Ctrl Pts',(11.0109275363277,0.176276582694249,15.8784425964261));
#6032=CARTESIAN_POINT('Ctrl Pts',(11.0225649861349,0.14226151080342,15.8901343381799));
#6033=CARTESIAN_POINT('Ctrl Pts',(11.0376188560823,0.0729388013115952,15.9046912409227));
#6034=CARTESIAN_POINT('Ctrl Pts',(11.0415308605551,0.0384029564419577,15.9081284852292));
#6035=CARTESIAN_POINT('Ctrl Pts',(11.0417998828598,0.00249739362048287,
15.9083716855965));
#6036=CARTESIAN_POINT('Ctrl Pts',(11.0418045603937,0.0012486595197422,15.9083759136321));
#6037=CARTESIAN_POINT('Ctrl Pts',(11.0418045603937,-2.17744741094999E-16,
15.9083759136321));
#6038=CARTESIAN_POINT('Origin',(10.5418045603937,0.,16.));
#6039=CARTESIAN_POINT('',(10.8667359346828,0.380025791233421,16.));
#6040=CARTESIAN_POINT('Origin',(12.8302991238869,0.,12.));
#6041=CARTESIAN_POINT('Origin',(12.8302991238869,0.,16.));
#6042=CARTESIAN_POINT('Origin',(12.8302991238869,0.,12.));
#6043=CARTESIAN_POINT('',(11.8302991238869,-1.22464679914735E-16,10.));
#6044=CARTESIAN_POINT('Origin',(12.8302991238869,0.,10.));
#6045=CARTESIAN_POINT('',(11.8302991238869,1.22464679914735E-16,12.));
#6046=CARTESIAN_POINT('Origin',(12.8302991238869,0.,10.));
#6047=CARTESIAN_POINT('',(0.,0.,0.));
#6048=CARTESIAN_POINT('Origin',(65.0333054217745,2.89627205572787,11.2802348949791));
#6049=CARTESIAN_POINT('',(40.4874595913632,1.99731386475336,10.8422004546896));
#6050=CARTESIAN_POINT('',(40.4874595913632,3.47301042256638,10.4633059774983));
#6051=CARTESIAN_POINT('Ctrl Pts',(40.4874595913632,1.99731386475335,10.8422004546896));
#6052=CARTESIAN_POINT('Ctrl Pts',(40.4362950734394,2.02504082610839,10.7852976709622));
#6053=CARTESIAN_POINT('Ctrl Pts',(40.3883369165899,2.05851119287108,10.7303891684628));
#6054=CARTESIAN_POINT('Ctrl Pts',(40.2799612282044,2.15565705872171,10.601352159818));
#6055=CARTESIAN_POINT('Ctrl Pts',(40.2177890646542,2.2340948035392,10.5221252828469));
#6056=CARTESIAN_POINT('Ctrl Pts',(40.1312057824654,2.42334768794107,10.391667759134));
#6057=CARTESIAN_POINT('Ctrl Pts',(40.107260046221,2.53453990097136,10.3406760550451));
#6058=CARTESIAN_POINT('Ctrl Pts',(40.107260046221,2.76062443615468,10.282627412656));
#6059=CARTESIAN_POINT('Ctrl Pts',(40.1312057824654,2.88262835599554,10.2737445264171));
#6060=CARTESIAN_POINT('Ctrl Pts',(40.2177890646542,3.11132031417736,10.2968920535137));
#6061=CARTESIAN_POINT('Ctrl Pts',(40.2799612282044,3.21822367299693,10.3285314232885));
#6062=CARTESIAN_POINT('Ctrl Pts',(40.3883369165899,3.3655172971902,10.3948070381394));
#6063=CARTESIAN_POINT('Ctrl Pts',(40.4362950734393,3.42129997598637,10.4267992535094));
#6064=CARTESIAN_POINT('Ctrl Pts',(40.4874595913632,3.47301042256638,10.4633059774983));
#6065=CARTESIAN_POINT('',(44.4440437425414,1.99731386475336,10.8422004546896));
#6066=CARTESIAN_POINT('',(65.0333054217745,1.99731386475335,10.8422004546896));
#6067=CARTESIAN_POINT('',(44.4440437425414,3.47301042256638,10.4633059774983));
#6068=CARTESIAN_POINT('Ctrl Pts',(44.4440437425414,3.47301042256638,10.4633059774983));
#6069=CARTESIAN_POINT('Ctrl Pts',(44.494558600482,3.42150132578768,10.4269414031543));
#6070=CARTESIAN_POINT('Ctrl Pts',(44.5419028922086,3.36596803166599,10.3950689245517));
#6071=CARTESIAN_POINT('Ctrl Pts',(44.6493790253187,3.21879552819819,10.3287004100455));
#6072=CARTESIAN_POINT('Ctrl Pts',(44.7111607127654,3.11169821280053,10.2969577118196));
#6073=CARTESIAN_POINT('Ctrl Pts',(44.7971423090715,2.8827215071592,10.2737266025933));
#6074=CARTESIAN_POINT('Ctrl Pts',(44.8208830494268,2.76063081774635,10.2826257741417));
#6075=CARTESIAN_POINT('Ctrl Pts',(44.8208830494268,2.53453351937968,10.3406776935593));
#6076=CARTESIAN_POINT('Ctrl Pts',(44.7971423090715,2.42325742408613,10.3916969282828));
#6077=CARTESIAN_POINT('Ctrl Pts',(44.7111607127654,2.23379527958143,10.5223648737091));
#6078=CARTESIAN_POINT('Ctrl Pts',(44.6493790253187,2.15523734817991,10.6017757373863));
#6079=CARTESIAN_POINT('Ctrl Pts',(44.5419028922086,2.05824237598036,10.7308358042651));
#6080=CARTESIAN_POINT('Ctrl Pts',(44.494558600482,2.0249328630462,10.7855192386522));
#6081=CARTESIAN_POINT('Ctrl Pts',(44.4440437425414,1.99731386475335,10.8422004546895));
#6082=CARTESIAN_POINT('',(65.0333054217745,3.47301042256639,10.4633059774983));
#6083=CARTESIAN_POINT('Origin',(65.0333054217745,5.61056068645085,10.2055720021147));
#6084=CARTESIAN_POINT('',(40.4874595913632,4.63091018458434,10.0048610303352));
#6085=CARTESIAN_POINT('',(40.4874595913632,5.96601779663743,9.270879409431));
#6086=CARTESIAN_POINT('Ctrl Pts',(40.4874595913632,4.63091018458433,10.0048610303352));
#6087=CARTESIAN_POINT('Ctrl Pts',(40.4362950734394,4.64361490559755,9.94285053730468));
#6088=CARTESIAN_POINT('Ctrl Pts',(40.3883369165899,4.66237854994973,9.88134334464741));
#6089=CARTESIAN_POINT('Ctrl Pts',(40.2799612282044,4.72438220066596,9.73220107649475));
#6090=CARTESIAN_POINT('Ctrl Pts',(40.2177890646542,4.78065275639872,9.63595658364359));
#6091=CARTESIAN_POINT('Ctrl Pts',(40.1312057824654,4.93151644657343,9.46253234446524));
#6092=CARTESIAN_POINT('Ctrl Pts',(40.107260046221,5.02653423062696,9.38549025961531));
#6093=CARTESIAN_POINT('Ctrl Pts',(40.107260046221,5.2310797940713,9.27304038452639));
#6094=CARTESIAN_POINT('Ctrl Pts',(40.1312057824654,5.34704165244441,9.23409542943431));
#6095=CARTESIAN_POINT('Ctrl Pts',(40.2177890646542,5.57430538812665,9.19964235712613));
#6096=CARTESIAN_POINT('Ctrl Pts',(40.2799612282044,5.68571857264663,9.20370193367626));
#6097=CARTESIAN_POINT('Ctrl Pts',(40.3883369165899,5.84486677196091,9.23126494343362));
#6098=CARTESIAN_POINT('Ctrl Pts',(40.4362950734394,5.90685307575603,9.24837947643258));
#6099=CARTESIAN_POINT('Ctrl Pts',(40.4874595913632,5.96601779663743,9.270879409431));
#6100=CARTESIAN_POINT('',(44.4440437425414,4.63091018458434,10.0048610303352));
#6101=CARTESIAN_POINT('',(65.0333054217746,4.63091018458433,10.0048610303352));
#6102=CARTESIAN_POINT('',(44.4440437425414,5.96601779663743,9.270879409431));
#6103=CARTESIAN_POINT('Ctrl Pts',(44.4440437425414,5.96601779663743,9.270879409431));
#6104=CARTESIAN_POINT('Ctrl Pts',(44.494558600482,5.90708345096223,9.24846708652567));
#6105=CARTESIAN_POINT('Ctrl Pts',(44.5419028922086,5.84536847428662,9.2314065090968));
#6106=CARTESIAN_POINT('Ctrl Pts',(44.6493790253187,5.68631448726271,9.20372339679809));
#6107=CARTESIAN_POINT('Ctrl Pts',(44.7111607127654,5.57468774292636,9.19961197308963));
#6108=CARTESIAN_POINT('Ctrl Pts',(44.7971423090715,5.34712741961925,9.23405490296801));
#6109=CARTESIAN_POINT('Ctrl Pts',(44.8208830494268,5.23108556769161,9.27303721045176));
#6110=CARTESIAN_POINT('Ctrl Pts',(44.8208830494268,5.02652845700665,9.38549343368993));
#6111=CARTESIAN_POINT('Ctrl Pts',(44.7971423090715,4.93143627259579,9.4625830449195));
#6112=CARTESIAN_POINT('Ctrl Pts',(44.7111607127654,4.78042222636135,9.63626313589754));
#6113=CARTESIAN_POINT('Ctrl Pts',(44.6493790253187,4.72408101556028,9.7327157243621));
#6114=CARTESIAN_POINT('Ctrl Pts',(44.5419028922086,4.66222925224323,9.88184280060689));
#6115=CARTESIAN_POINT('Ctrl Pts',(44.494558600482,4.64356543603732,9.94309199336003));
#6116=CARTESIAN_POINT('Ctrl Pts',(44.4440437425414,4.63091018458433,10.0048610303352));
#6117=CARTESIAN_POINT('',(65.0333054217746,5.96601779663744,9.270879409431));
#6118=CARTESIAN_POINT('Origin',(65.0333054217745,7.97231715504529,8.48965548688909));
#6119=CARTESIAN_POINT('',(40.4874595913632,6.97352938622157,8.53887939213984));
#6120=CARTESIAN_POINT('',(40.4874595913632,8.08415833106712,7.49592939215974));
#6121=CARTESIAN_POINT('Ctrl Pts',(40.4874595913632,6.97352938622157,8.53887939213984));
#6122=CARTESIAN_POINT('Ctrl Pts',(40.4362950734394,6.97041358254702,8.47565753714199));
#6123=CARTESIAN_POINT('Ctrl Pts',(40.3883369165899,6.97329151570619,8.41141637744912));
#6124=CARTESIAN_POINT('Ctrl Pts',(40.2799612282044,6.99625703388003,8.25154000700349));
#6125=CARTESIAN_POINT('Ctrl Pts',(40.2177890646542,7.02682471456273,8.14432529372061));
#6126=CARTESIAN_POINT('Ctrl Pts',(40.1312057824654,7.12981989001876,7.93883122183409));
#6127=CARTESIAN_POINT('Ctrl Pts',(40.107260046221,7.2026929282725,7.84057959375527));
#6128=CARTESIAN_POINT('Ctrl Pts',(40.107260046221,7.37284716996069,7.68079412518009));
#6129=CARTESIAN_POINT('Ctrl Pts',(40.1312057824654,7.47548065682658,7.61423415599275));
#6130=CARTESIAN_POINT('Ctrl Pts',(40.2177890646542,7.68703635367878,7.52434529752242));
#6131=CARTESIAN_POINT('Ctrl Pts',(40.2799612282044,7.79595886376674,7.50057000272324));
#6132=CARTESIAN_POINT('Ctrl Pts',(40.3883369165899,7.95696177153297,7.48768852211428));
#6133=CARTESIAN_POINT('Ctrl Pts',(40.4362950734394,8.02125687288992,7.48885000369109));
#6134=CARTESIAN_POINT('Ctrl Pts',(40.4874595913632,8.08415833106712,7.49592939215974));
#6135=CARTESIAN_POINT('',(44.4440437425414,6.97352938622157,8.53887939213984));
#6136=CARTESIAN_POINT('',(65.0333054217745,6.97352938622157,8.53887939213985));
#6137=CARTESIAN_POINT('',(44.4440437425414,8.08415833106712,7.49592939215974));
#6138=CARTESIAN_POINT('Ctrl Pts',(44.4440437425414,8.08415833106712,7.49592939215974));
#6139=CARTESIAN_POINT('Ctrl Pts',(44.494558600482,8.02150179817957,7.48887756936796));
#6140=CARTESIAN_POINT('Ctrl Pts',(44.5419028922086,7.95748291790636,7.48770087193706));
#6141=CARTESIAN_POINT('Ctrl Pts',(44.6493790253187,7.79654139429069,7.500442593603));
#6142=CARTESIAN_POINT('Ctrl Pts',(44.7111607127654,7.68739913989674,7.52422078028431));
#6143=CARTESIAN_POINT('Ctrl Pts',(44.7971423090715,7.47555365094558,7.61417357331088));
#6144=CARTESIAN_POINT('Ctrl Pts',(44.8208830494268,7.37285197283185,7.68078961498387));
#6145=CARTESIAN_POINT('Ctrl Pts',(44.8208830494268,7.20268812540135,7.8405841039515));
#6146=CARTESIAN_POINT('Ctrl Pts',(44.7971423090715,7.12975484354432,7.9389002678978));
#6147=CARTESIAN_POINT('Ctrl Pts',(44.7111607127654,7.02667766349585,8.14467954556077));
#6148=CARTESIAN_POINT('Ctrl Pts',(44.6493790253187,6.99609329877835,8.25211338795166));
#6149=CARTESIAN_POINT('Ctrl Pts',(44.5419028922086,6.97327111810788,8.41193727091097));
#6150=CARTESIAN_POINT('Ctrl Pts',(44.494558600482,6.97042571484315,8.47590370999069));
#6151=CARTESIAN_POINT('Ctrl Pts',(44.4440437425414,6.97352938622157,8.53887939213984));
#6152=CARTESIAN_POINT('',(65.0333054217745,8.08415833106713,7.49592939215974));
#6153=CARTESIAN_POINT('Origin',(65.0333054217745,9.83314361665672,6.24030269465341));
#6154=CARTESIAN_POINT('',(40.4874595913632,8.87797608967546,6.53636855793469));
#6155=CARTESIAN_POINT('',(40.4874595913632,9.69434146610128,5.2499825630792));
#6156=CARTESIAN_POINT('Ctrl Pts',(40.4874595913632,8.87797608967545,6.53636855793469));
#6157=CARTESIAN_POINT('Ctrl Pts',(40.4362950734394,8.85923553871713,6.47590780263271));
#6158=CARTESIAN_POINT('Ctrl Pts',(40.3883369165899,8.84604692955859,6.41296918423019));
#6159=CARTESIAN_POINT('Ctrl Pts',(40.2799612282044,8.82853130722192,6.25240433183086));
#6160=CARTESIAN_POINT('Ctrl Pts',(40.2177890646542,8.83147543305721,6.14095609285996));
#6161=CARTESIAN_POINT('Ctrl Pts',(40.1312057824654,8.88013052813091,5.91630413655623));
#6162=CARTESIAN_POINT('Ctrl Pts',(40.107260046221,8.92627993958308,5.80301647638493));
#6163=CARTESIAN_POINT('Ctrl Pts',(40.107260046221,9.05135144272633,5.6059353229639));
#6164=CARTESIAN_POINT('Ctrl Pts',(40.1312057824654,9.13420771864564,5.51594254733579));
#6165=CARTESIAN_POINT('Ctrl Pts',(40.2177890646542,9.31676255418716,5.3762659502691));
#6166=CARTESIAN_POINT('Ctrl Pts',(40.2799612282044,9.4163503879453,5.32614967333226));
#6167=CARTESIAN_POINT('Ctrl Pts',(40.3883369165899,9.56909159934126,5.27363309315842));
#6168=CARTESIAN_POINT('Ctrl Pts',(40.4362950734394,9.63165560058094,5.25876854315396));
#6169=CARTESIAN_POINT('Ctrl Pts',(40.4874595913632,9.69434146610128,5.24998256307919));
#6170=CARTESIAN_POINT('',(44.4440437425414,8.87797608967546,6.53636855793469));
#6171=CARTESIAN_POINT('',(65.0333054217745,8.87797608967545,6.5363685579347));
#6172=CARTESIAN_POINT('',(44.4440437425414,9.69434146610128,5.2499825630792));
#6173=CARTESIAN_POINT('Ctrl Pts',(44.4440437425414,9.69434146610128,5.24998256307919));
#6174=CARTESIAN_POINT('Ctrl Pts',(44.494558600482,9.6318996863973,5.25873433236176));
#6175=CARTESIAN_POINT('Ctrl Pts',(44.5419028922086,9.56959944421904,5.27351545115601));
#6176=CARTESIAN_POINT('Ctrl Pts',(44.6493790253187,9.4168829318419,5.32588139755355));
#6177=CARTESIAN_POINT('Ctrl Pts',(44.7111607127654,9.31708297663106,5.37605512370539));
#6178=CARTESIAN_POINT('Ctrl Pts',(44.7971423090715,9.13426335321984,5.51586571507106));
#6179=CARTESIAN_POINT('Ctrl Pts',(44.8208830494268,9.05135497306626,5.6059297600383));
#6180=CARTESIAN_POINT('Ctrl Pts',(44.8208830494268,8.92627640924314,5.80302203931053));
#6181=CARTESIAN_POINT('Ctrl Pts',(44.7971423090715,8.88008469626887,5.91638718981127));
#6182=CARTESIAN_POINT('Ctrl Pts',(44.7111607127654,8.83142110072016,6.14133578534036));
#6183=CARTESIAN_POINT('Ctrl Pts',(44.6493790253187,8.82851531020285,6.25300041822613));
#6184=CARTESIAN_POINT('Ctrl Pts',(44.5419028922086,8.8461567137246,6.41347878554251));
#6185=CARTESIAN_POINT('Ctrl Pts',(44.494558600482,8.85930851055284,6.47614322432933));
#6186=CARTESIAN_POINT('Ctrl Pts',(44.4440437425414,8.87797608967545,6.53636855793469));
#6187=CARTESIAN_POINT('',(65.0333054217745,9.69434146610128,5.24998256307919));
#6188=CARTESIAN_POINT('Origin',(65.0333054217745,11.0761175010611,3.59884873388474));
#6189=CARTESIAN_POINT('',(40.4874595913632,10.2245869045029,4.1231536481525));
#6190=CARTESIAN_POINT('',(40.4874595913632,10.6953934735264,2.67416002147514));
#6191=CARTESIAN_POINT('Ctrl Pts',(40.4874595913632,10.2245869045029,4.12315364815251));
#6192=CARTESIAN_POINT('Ctrl Pts',(40.4362950734394,10.1913991440005,4.06925296416111));
#6193=CARTESIAN_POINT('Ctrl Pts',(40.3883369165899,10.162972681342,4.01157155191524));
#6194=CARTESIAN_POINT('Ctrl Pts',(40.2799612282044,10.1060764894642,3.86040709775467));
#6195=CARTESIAN_POINT('Ctrl Pts',(40.2177890646542,10.0812120701981,3.75172803582823));
#6196=CARTESIAN_POINT('Ctrl Pts',(40.1312057824654,10.072469906325,3.52203390373397));
#6197=CARTESIAN_POINT('Ctrl Pts',(40.107260046221,10.0889959537284,3.40082849180162));
#6198=CARTESIAN_POINT('Ctrl Pts',(40.107260046221,10.1611260158034,3.17883498721797));
#6199=CARTESIAN_POINT('Ctrl Pts',(40.1312057824654,10.2189989162361,3.07106398221208));
#6200=CARTESIAN_POINT('Ctrl Pts',(40.2177890646542,10.3610822987601,2.89037604083731));
#6201=CARTESIAN_POINT('Ctrl Pts',(40.2799612282044,10.445077986335,2.81706777175753));
#6202=CARTESIAN_POINT('Ctrl Pts',(40.3883369165899,10.5799602093058,2.7282159018936));
#6203=CARTESIAN_POINT('Ctrl Pts',(40.4362950734394,10.636861984136,2.69825931465265));
#6204=CARTESIAN_POINT('Ctrl Pts',(40.4874595913632,10.6953934735264,2.67416002147513));
#6205=CARTESIAN_POINT('',(44.4440437425414,10.2245869045029,4.1231536481525));
#6206=CARTESIAN_POINT('',(65.0333054217745,10.2245869045029,4.12315364815251));
#6207=CARTESIAN_POINT('',(44.4440437425414,10.6953934735264,2.67416002147514));
#6208=CARTESIAN_POINT('Ctrl Pts',(44.4440437425414,10.6953934735264,2.67416002147513));
#6209=CARTESIAN_POINT('Ctrl Pts',(44.494558600482,10.6370898936696,2.69816547698127));
#6210=CARTESIAN_POINT('Ctrl Pts',(44.5419028922086,10.5804228429266,2.72797565994567));
#6211=CARTESIAN_POINT('Ctrl Pts',(44.6493790253187,10.4455270819127,2.81667548607418));
#6212=CARTESIAN_POINT('Ctrl Pts',(44.7111607127654,10.3613402241094,2.89009215195636));
#6213=CARTESIAN_POINT('Ctrl Pts',(44.7971423090715,10.2190336955406,3.07097572801825));
#6214=CARTESIAN_POINT('Ctrl Pts',(44.8208830494268,10.1611280517879,3.17882872110207));
#6215=CARTESIAN_POINT('Ctrl Pts',(44.8208830494268,10.088993917744,3.40083475791752));
#6216=CARTESIAN_POINT('Ctrl Pts',(44.7971423090715,10.0724461688598,3.52212574563888));
#6217=CARTESIAN_POINT('Ctrl Pts',(44.7111607127654,10.0812538704914,3.75210931147394));
#6218=CARTESIAN_POINT('Ctrl Pts',(44.6493790253187,10.1062092356792,3.86098843529658));
#6219=CARTESIAN_POINT('Ctrl Pts',(44.5419028922086,10.1632057491294,4.01203784095338));
#6220=CARTESIAN_POINT('Ctrl Pts',(44.494558600482,10.191528370287,4.06946284229465));
#6221=CARTESIAN_POINT('Ctrl Pts',(44.4440437425414,10.2245869045029,4.12315364815251));
#6222=CARTESIAN_POINT('',(65.0333054217745,10.6953934735264,2.67416002147513));
#6223=CARTESIAN_POINT('Origin',(65.0333054217745,11.6231381877631,0.731265871526308));
#6224=CARTESIAN_POINT('',(40.4874595913632,10.9287493207203,1.45086583075851));
#6225=CARTESIAN_POINT('',(40.4874595913632,11.0244145741041,-0.0696898291507925));
#6226=CARTESIAN_POINT('Ctrl Pts',(40.4874595913632,10.9287493207203,1.45086583075852));
#6227=CARTESIAN_POINT('Ctrl Pts',(40.4362950734394,10.8831996597221,1.40691199628575));
#6228=CARTESIAN_POINT('Ctrl Pts',(40.3883369165899,10.8413214827577,1.35811212546531));
#6229=CARTESIAN_POINT('Ctrl Pts',(40.2799612282044,10.7486197183239,1.22584628814239));
#6230=CARTESIAN_POINT('Ctrl Pts',(40.2177890646542,10.6975090768639,1.12676510841489));
#6231=CARTESIAN_POINT('Ctrl Pts',(40.1312057824654,10.6319189563517,0.906461327605495));
#6232=CARTESIAN_POINT('Ctrl Pts',(40.107260046221,10.6177832473694,0.784953945706135));
#6233=CARTESIAN_POINT('Ctrl Pts',(40.107260046221,10.6324396713002,0.551996758287852));
#6234=CARTESIAN_POINT('Ctrl Pts',(40.1312057824654,10.6616928290704,0.433219172502737));
#6235=CARTESIAN_POINT('Ctrl Pts',(40.2177890646542,10.7543771371068,0.222873174700238));
#6236=CARTESIAN_POINT('Ctrl Pts',(40.2799612282044,10.8175029205336,0.130979141632741));
#6237=CARTESIAN_POINT('Ctrl Pts',(40.3883369165899,10.9260510089478,0.0113748718365951));
#6238=CARTESIAN_POINT('Ctrl Pts',(40.4362950734394,10.9737152095859,-0.0317914700918793));
#6239=CARTESIAN_POINT('Ctrl Pts',(40.4874595913632,11.0244145741041,-0.0696898291507991));
#6240=CARTESIAN_POINT('',(44.4440437425414,10.9287493207203,1.45086583075851));
#6241=CARTESIAN_POINT('',(65.0333054217745,10.9287493207203,1.45086583075852));
#6242=CARTESIAN_POINT('',(44.4440437425414,11.0244145741041,-0.0696898291507925));
#6243=CARTESIAN_POINT('Ctrl Pts',(44.4440437425414,11.0244145741041,-0.0696898291507991));
#6244=CARTESIAN_POINT('Ctrl Pts',(44.494558600482,10.9739126224425,-0.0319390384764372));
#6245=CARTESIAN_POINT('Ctrl Pts',(44.5419028922086,10.9264393623398,0.0110271252282886));
#6246=CARTESIAN_POINT('Ctrl Pts',(44.6493790253187,10.8178403494655,0.130487494796957));
#6247=CARTESIAN_POINT('Ctrl Pts',(44.7111607127654,10.7545563589632,0.222534061284509));
#6248=CARTESIAN_POINT('Ctrl Pts',(44.7971423090715,10.6617045677936,0.43312504171538));
#6249=CARTESIAN_POINT('Ctrl Pts',(44.8208830494268,10.6324400850008,0.551990182704755));
#6250=CARTESIAN_POINT('Ctrl Pts',(44.8208830494268,10.6177828336688,0.784960521289232));
#6251=CARTESIAN_POINT('Ctrl Pts',(44.7971423090715,10.6319188047956,0.906556187395616));
#6252=CARTESIAN_POINT('Ctrl Pts',(44.7111607127654,10.6976443833215,1.12712401027484));
#6253=CARTESIAN_POINT('Ctrl Pts',(44.6493790253187,10.7488928668403,1.22637634925516));
#6254=CARTESIAN_POINT('Ctrl Pts',(44.5419028922086,10.8416631896602,1.35850580357412));
#6255=CARTESIAN_POINT('Ctrl Pts',(44.494558600482,10.8833770206965,1.40708314344118));
#6256=CARTESIAN_POINT('Ctrl Pts',(44.4440437425414,10.9287493207203,1.45086583075852));
#6257=CARTESIAN_POINT('',(65.0333054217745,11.0244145741041,-0.0696898291508022));
#6258=CARTESIAN_POINT('Origin',(65.0333054217745,11.4398343552159,-2.18226511494788));
#6259=CARTESIAN_POINT('',(40.4874595913632,10.9462182239883,-1.31258522269331));
#6260=CARTESIAN_POINT('',(40.4874595913632,10.6607311620303,-2.80916081150993));
#6261=CARTESIAN_POINT('Ctrl Pts',(40.4874595913632,10.9462182239883,-1.3125852226933));
#6262=CARTESIAN_POINT('Ctrl Pts',(40.4362950734394,10.8911687152148,-1.34383042657663));
#6263=CARTESIAN_POINT('Ctrl Pts',(40.3883369165899,10.8384701838204,-1.38068248061461));
#6264=CARTESIAN_POINT('Ctrl Pts',(40.2799612282044,10.7157876396233,-1.48573895210117));
#6265=CARTESIAN_POINT('Ctrl Pts',(40.2177890646542,10.6416422455441,-1.56899661471235));
#6266=CARTESIAN_POINT('Ctrl Pts',(40.1312057824654,10.5233254368881,-1.766067547468));
#6267=CARTESIAN_POINT('Ctrl Pts',(40.107260046221,10.479416170103,-1.88024214365675));
#6268=CARTESIAN_POINT('Ctrl Pts',(40.107260046221,10.4356780388714,-2.10952545706757));
#6269=CARTESIAN_POINT('Ctrl Pts',(40.1312057824654,10.4344733704908,-2.23184639108363));
#6270=CARTESIAN_POINT('Ctrl Pts',(40.2177890646542,10.4719349080967,-2.45863363267346));
#6271=CARTESIAN_POINT('Ctrl Pts',(40.2799612282044,10.5102243622422,-2.56333938966843));
#6272=CARTESIAN_POINT('Ctrl Pts',(40.3883369165899,10.5856178404929,-2.70618088325176));
#6273=CARTESIAN_POINT('Ctrl Pts',(40.4362950734393,10.6210495499161,-2.75984467984969));
#6274=CARTESIAN_POINT('Ctrl Pts',(40.4874595913632,10.6607311620303,-2.80916081150993));
#6275=CARTESIAN_POINT('',(44.4440437425414,10.9462182239883,-1.31258522269331));
#6276=CARTESIAN_POINT('',(65.0333054217745,10.9462182239883,-1.3125852226933));
#6277=CARTESIAN_POINT('',(44.4440437425414,10.6607311620303,-2.80916081150993));
#6278=CARTESIAN_POINT('Ctrl Pts',(44.4440437425414,10.6607311620303,-2.80916081150993));
#6279=CARTESIAN_POINT('Ctrl Pts',(44.494558600482,10.6212040619198,-2.76003670668311));
#6280=CARTESIAN_POINT('Ctrl Pts',(44.5419028922086,10.5859075119841,-2.70661428432213));
#6281=CARTESIAN_POINT('Ctrl Pts',(44.6493790253187,10.5104289226276,-2.5638995056778));
#6282=CARTESIAN_POINT('Ctrl Pts',(44.7111607127654,10.4720241652918,-2.45900666288089));
#6283=CARTESIAN_POINT('Ctrl Pts',(44.7971423090715,10.4344613310455,-2.23194048388096));
#6284=CARTESIAN_POINT('Ctrl Pts',(44.8208830494268,10.4356768042938,-2.10953192894979));
#6285=CARTESIAN_POINT('Ctrl Pts',(44.8208830494268,10.4794174046805,-1.88023567177453));
#6286=CARTESIAN_POINT('Ctrl Pts',(44.7971423090715,10.5233488807639,-1.76597563018215));
#6287=CARTESIAN_POINT('Ctrl Pts',(44.7111607127654,10.6418625563635,-1.56868263776198));
#6288=CARTESIAN_POINT('Ctrl Pts',(44.6493790253187,10.7161840275151,-1.48529347310667));
#6289=CARTESIAN_POINT('Ctrl Pts',(44.5419028922086,10.8388990591367,-1.38038614967855));
#6290=CARTESIAN_POINT('Ctrl Pts',(44.494558600482,10.8913830666349,-1.34370876420452));
#6291=CARTESIAN_POINT('Ctrl Pts',(44.4440437425414,10.9462182239883,-1.3125852226933));
#6292=CARTESIAN_POINT('',(65.0333054217745,10.6607311620303,-2.80916081150994));
#6293=CARTESIAN_POINT('Origin',(65.0333054217745,10.5377236573627,-4.95867635844021));
#6294=CARTESIAN_POINT('',(40.4874595913632,10.2758959788686,-3.99356171925254));
#6295=CARTESIAN_POINT('',(40.4874595913632,9.62719480361945,-5.37212188871111));
#6296=CARTESIAN_POINT('Ctrl Pts',(40.4874595913632,10.2758959788686,-3.99356171925253));
#6297=CARTESIAN_POINT('Ctrl Pts',(40.4362950734394,10.214805585414,-4.0101350414746));
#6298=CARTESIAN_POINT('Ctrl Pts',(40.3883369165899,10.1545979421286,-4.03272372864254));
#6299=CARTESIAN_POINT('Ctrl Pts',(40.2799612282044,10.009643213615,-4.10396974981855));
#6300=CARTESIAN_POINT('Ctrl Pts',(40.2177890646542,9.9171218947142,-4.16617251017131));
#6301=CARTESIAN_POINT('Ctrl Pts',(40.1312057824654,9.75351267814105,-4.32762790339198));
#6302=CARTESIAN_POINT('Ctrl Pts',(40.107260046221,9.68258883427222,-4.42729570408678));
#6303=CARTESIAN_POINT('Ctrl Pts',(40.107260046221,9.58320437552114,-4.63849842966349));
#6304=CARTESIAN_POINT('Ctrl Pts',(40.1312057824654,9.55161757473464,-4.75667683776135));
#6305=CARTESIAN_POINT('Ctrl Pts',(40.2177890646542,9.53150249572827,-4.9856554466843));
#6306=CARTESIAN_POINT('Ctrl Pts',(40.2799612282044,9.54254975336982,-5.09659387981389));
#6307=CARTESIAN_POINT('Ctrl Pts',(40.3883369165899,9.58005137194069,-5.25369734080832));
#6308=CARTESIAN_POINT('Ctrl Pts',(40.4362950734393,9.60102428553722,-5.31448669837381));
#6309=CARTESIAN_POINT('Ctrl Pts',(40.4874595913632,9.62719480361944,-5.37212188871111));
#6310=CARTESIAN_POINT('',(44.4440437425414,10.2758959788686,-3.99356171925254));
#6311=CARTESIAN_POINT('',(65.0333054217745,10.2758959788686,-3.99356171925253));
#6312=CARTESIAN_POINT('',(44.4440437425414,9.62719480361945,-5.37212188871111));
#6313=CARTESIAN_POINT('Ctrl Pts',(44.4440437425414,9.62719480361944,-5.37212188871111));
#6314=CARTESIAN_POINT('Ctrl Pts',(44.494558600482,9.6011261881307,-5.31471111790392));
#6315=CARTESIAN_POINT('Ctrl Pts',(44.5419028922086,9.58022416040606,-5.25418916415755));
#6316=CARTESIAN_POINT('Ctrl Pts',(44.6493790253187,9.54260859192743,-5.09718727084803));
#6317=CARTESIAN_POINT('Ctrl Pts',(44.7111607127654,9.53149617990425,-4.98603895482358));
#6318=CARTESIAN_POINT('Ctrl Pts',(44.7971423090715,9.55158251360353,-4.75676498037213));
#6319=CARTESIAN_POINT('Ctrl Pts',(44.8208830494268,9.58320157023845,-4.63850439119268));
#6320=CARTESIAN_POINT('Ctrl Pts',(44.8208830494268,9.68259163955492,-4.42728974255759));
#6321=CARTESIAN_POINT('Ctrl Pts',(44.7971423090715,9.75355824438383,-4.32754470411152));
#6322=CARTESIAN_POINT('Ctrl Pts',(44.7111607127654,9.91741336695648,-4.16592318645703));
#6323=CARTESIAN_POINT('Ctrl Pts',(44.6493790253187,10.0101379343731,-4.10363684402592));
#6324=CARTESIAN_POINT('Ctrl Pts',(44.5419028922086,10.1550870380453,-4.03254336444178));
#6325=CARTESIAN_POINT('Ctrl Pts',(44.494558600482,10.2150434587916,-4.01007050838009));
#6326=CARTESIAN_POINT('Ctrl Pts',(44.4440437425414,10.2758959788686,-3.99356171925253));
#6327=CARTESIAN_POINT('',(65.0333054217745,9.62719480361944,-5.37212188871111));
#6328=CARTESIAN_POINT('Origin',(65.0333054217745,8.9734890270808,-7.42351572959578));
#6329=CARTESIAN_POINT('',(40.4874595913632,8.9599013972947,-6.42360804569852));
#6330=CARTESIAN_POINT('',(40.4874595913632,7.98874638935144,-7.59753279036232));
#6331=CARTESIAN_POINT('Ctrl Pts',(40.4874595913632,8.9599013972947,-6.42360804569851));
#6332=CARTESIAN_POINT('Ctrl Pts',(40.4362950734394,8.89660865325455,-6.42446812347171));
#6333=CARTESIAN_POINT('Ctrl Pts',(40.3883369165899,8.83267496573407,-6.43137411347946));
#6334=CARTESIAN_POINT('Ctrl Pts',(40.2799612282044,8.67455609160262,-6.46433303480991));
#6335=CARTESIAN_POINT('Ctrl Pts',(40.2177890646542,8.56947230261642,-6.50157246470552));
#6336=CARTESIAN_POINT('Ctrl Pts',(40.1312057824654,8.370850846916,-6.61726748224375));
#6337=CARTESIAN_POINT('Ctrl Pts',(40.107260046221,8.27736883191338,-6.69616599297443));
#6338=CARTESIAN_POINT('Ctrl Pts',(40.107260046221,8.12858273669663,-6.87601748671975));
#6339=CARTESIAN_POINT('Ctrl Pts',(40.1312057824654,8.06859851836572,-6.98262778488883));
#6340=CARTESIAN_POINT('Ctrl Pts',(40.2177890646542,7.99217072713916,-7.19941019302185));
#6341=CARTESIAN_POINT('Ctrl Pts',(40.2799612282044,7.97528164845017,-7.30961063252953));
#6342=CARTESIAN_POINT('Ctrl Pts',(40.3883369165899,7.97253504272508,-7.47110467269465));
#6343=CARTESIAN_POINT('Ctrl Pts',(40.4362950734393,7.97773135520069,-7.53519997232425));
#6344=CARTESIAN_POINT('Ctrl Pts',(40.4874595913632,7.98874638935144,-7.59753279036232));
#6345=CARTESIAN_POINT('',(44.4440437425414,8.9599013972947,-6.42360804569852));
#6346=CARTESIAN_POINT('',(65.0333054217745,8.95990139729471,-6.42360804569851));
#6347=CARTESIAN_POINT('',(44.4440437425414,7.98874638935144,-7.59753279036232));
#6348=CARTESIAN_POINT('Ctrl Pts',(44.4440437425414,7.98874638935144,-7.59753279036232));
#6349=CARTESIAN_POINT('Ctrl Pts',(44.494558600482,7.97777424546919,-7.53544268344662));
#6350=CARTESIAN_POINT('Ctrl Pts',(44.5419028922086,7.97258009122984,-7.47162401525292));
#6351=CARTESIAN_POINT('Ctrl Pts',(44.6493790253187,7.97519106813697,-7.31020001364741));
#6352=CARTESIAN_POINT('Ctrl Pts',(44.7111607127654,7.99206923514248,-7.19978008186615));
#6353=CARTESIAN_POINT('Ctrl Pts',(44.7971423090715,8.06854263856859,-6.98270443898868));
#6354=CARTESIAN_POINT('Ctrl Pts',(44.8208830494268,8.12857853697502,-6.87602256331111));
#6355=CARTESIAN_POINT('Ctrl Pts',(44.8208830494268,8.27737303163499,-6.69616091638308));
#6356=CARTESIAN_POINT('Ctrl Pts',(44.7971423090715,8.37091567243115,-6.61719822868546));
#6357=CARTESIAN_POINT('Ctrl Pts',(44.7111607127654,8.5698166220086,-6.50140346015324));
#6358=CARTESIAN_POINT('Ctrl Pts',(44.6493790253187,8.67511806010238,-6.46413361991442));
#6359=CARTESIAN_POINT('Ctrl Pts',(44.5419028922086,8.83319355055587,-6.43132104896007));
#6360=CARTESIAN_POINT('Ctrl Pts',(44.494558600482,8.89685510213054,-6.42446477450645));
#6361=CARTESIAN_POINT('Ctrl Pts',(44.4440437425414,8.9599013972947,-6.42360804569851));
#6362=CARTESIAN_POINT('',(65.0333054217745,7.98874638935144,-7.59753279036232));
#6363=CARTESIAN_POINT('Origin',(65.0333054217745,6.8454170790433,-9.42190830567978));
#6364=CARTESIAN_POINT('',(40.4874595913632,7.08092325871652,-8.45003545425543));
#6365=CARTESIAN_POINT('',(40.4874595913632,5.84833565888647,-9.34556276502401));
#6366=CARTESIAN_POINT('Ctrl Pts',(40.4874595913632,7.08092325871652,-8.45003545425542));
#6367=CARTESIAN_POINT('Ctrl Pts',(40.4362950734394,7.01940507997324,-8.4351282457301));
#6368=CARTESIAN_POINT('Ctrl Pts',(40.3883369165899,6.95576253693625,-8.42591760982703));
#6369=CARTESIAN_POINT('Ctrl Pts',(40.2799612282044,6.79441470756918,-8.41851850107028));
#6370=CARTESIAN_POINT('Ctrl Pts',(40.2177890646542,6.68337124943072,-8.42845471017137));
#6371=CARTESIAN_POINT('Ctrl Pts',(40.1312057824654,6.46221767114332,-8.49111980857872));
#6372=CARTESIAN_POINT('Ctrl Pts',(40.107260046221,6.35205130381232,-8.54429154574763));
#6373=CARTESIAN_POINT('Ctrl Pts',(40.107260046221,6.16321234968933,-8.68149107686204));
#6374=CARTESIAN_POINT('Ctrl Pts',(40.1312057824654,6.07859974285827,-8.76983454798312));
#6375=CARTESIAN_POINT('Ctrl Pts',(40.2177890646542,5.95066147861605,-8.96079951935329));
#6376=CARTESIAN_POINT('Ctrl Pts',(40.2799612282044,5.90689726652424,-9.06333766633592));
#6377=CARTESIAN_POINT('Ctrl Pts',(40.3883369165899,5.86407501584219,-9.21907502119462));
#6378=CARTESIAN_POINT('Ctrl Pts',(40.4362950734394,5.85316822377335,-9.28244891948659));
#6379=CARTESIAN_POINT('Ctrl Pts',(40.4874595913632,5.84833565888646,-9.34556276502401));
#6380=CARTESIAN_POINT('',(44.4440437425414,7.08092325871652,-8.45003545425543));
#6381=CARTESIAN_POINT('',(65.0333054217745,7.08092325871653,-8.45003545425542));
#6382=CARTESIAN_POINT('',(44.4440437425414,5.84833565888647,-9.34556276502401));
#6383=CARTESIAN_POINT('Ctrl Pts',(44.4440437425414,5.84833565888646,-9.34556276502401));
#6384=CARTESIAN_POINT('Ctrl Pts',(44.494558600482,5.85314940676356,-9.28269467176876));
#6385=CARTESIAN_POINT('Ctrl Pts',(44.5419028922086,5.86398949382312,-9.21958925075899));
#6386=CARTESIAN_POINT('Ctrl Pts',(44.6493790253187,5.90666295883444,-9.06388600455431));
#6387=CARTESIAN_POINT('Ctrl Pts',(44.7111607127654,5.95047118756212,-8.96113254742616));
#6388=CARTESIAN_POINT('Ctrl Pts',(44.7971423090715,6.07852655552828,-8.76989489711302));
#6389=CARTESIAN_POINT('Ctrl Pts',(44.8208830494268,6.16320701941278,-8.68149494953464));
#6390=CARTESIAN_POINT('Ctrl Pts',(44.8208830494268,6.35205663408888,-8.54428767307503));
#6391=CARTESIAN_POINT('Ctrl Pts',(44.7971423090715,6.46229768270531,-8.49106885219836));
#6392=CARTESIAN_POINT('Ctrl Pts',(44.7111607127654,6.68374678111908,-8.42837664395866));
#6393=CARTESIAN_POINT('Ctrl Pts',(44.6493790253187,6.79500861326298,-8.41846510704323));
#6394=CARTESIAN_POINT('Ctrl Pts',(44.5419028922086,6.9562780260716,-8.42599517922791));
#6395=CARTESIAN_POINT('Ctrl Pts',(44.494558600482,7.01964461905841,-8.43518629132191));
#6396=CARTESIAN_POINT('Ctrl Pts',(44.4440437425414,7.08092325871652,-8.45003545425542));
#6397=CARTESIAN_POINT('',(65.0333054217745,5.84833565888646,-9.34556276502402));
#6398=CARTESIAN_POINT('Origin',(65.0333054217745,4.28722240024657,-10.8282877315631));
#6399=CARTESIAN_POINT('',(40.4874595913632,4.75702466997909,-9.94551605816494));
#6400=CARTESIAN_POINT('',(40.4874595913632,3.34045249029966,-10.5063766605837));
#6401=CARTESIAN_POINT('Ctrl Pts',(40.4874595913632,4.7570246699791,-9.94551605816493));
#6402=CARTESIAN_POINT('Ctrl Pts',(40.4362950734394,4.70114646995116,-9.91577823807761));
#6403=CARTESIAN_POINT('Ctrl Pts',(40.3883369165899,4.64179396643758,-9.89102971439186));
#6404=CARTESIAN_POINT('Ctrl Pts',(40.2799612282044,4.48735525934981,-9.84373748876312));
#6405=CARTESIAN_POINT('Ctrl Pts',(40.2177890646542,4.37732940092321,-9.82574614850904));
#6406=CARTESIAN_POINT('Ctrl Pts',(40.1312057824654,4.1475395927186,-9.83144384918648));
#6407=CARTESIAN_POINT('Ctrl Pts',(40.107260046221,4.02761103108218,-9.85554783699533));
#6408=CARTESIAN_POINT('Ctrl Pts',(40.107260046221,3.8105846640416,-9.94147465435431));
#6409=CARTESIAN_POINT('Ctrl Pts',(40.1312057824654,3.70666018998099,-10.0060003532323));
#6410=CARTESIAN_POINT('Ctrl Pts',(40.2177890646542,3.53525028438945,-10.1591488563684));
#6411=CARTESIAN_POINT('Ctrl Pts',(40.2799612282044,3.46736080529406,-10.2475818619421));
#6412=CARTESIAN_POINT('Ctrl Pts',(40.3883369165899,3.38715358915463,-10.3877769807267));
#6413=CARTESIAN_POINT('Ctrl Pts',(40.4362950734393,3.3608290063994,-10.4464474625785));
#6414=CARTESIAN_POINT('Ctrl Pts',(40.4874595913632,3.34045249029966,-10.5063766605837));
#6415=CARTESIAN_POINT('',(44.4440437425414,4.75702466997909,-9.94551605816494));
#6416=CARTESIAN_POINT('',(65.0333054217745,4.7570246699791,-9.94551605816493));
#6417=CARTESIAN_POINT('',(44.4440437425414,3.34045249029966,-10.5063766605837));
#6418=CARTESIAN_POINT('Ctrl Pts',(44.4440437425414,3.34045249029966,-10.5063766605837));
#6419=CARTESIAN_POINT('Ctrl Pts',(44.494558600482,3.36074966445325,-10.4466808145007));
#6420=CARTESIAN_POINT('Ctrl Pts',(44.5419028922086,3.38694287027472,-10.3882537863625));
#6421=CARTESIAN_POINT('Ctrl Pts',(44.6493790253187,3.46699749264154,-10.2480547031541));
#6422=CARTESIAN_POINT('Ctrl Pts',(44.7111607127654,3.53498315096504,-10.1594240982912));
#6423=CARTESIAN_POINT('Ctrl Pts',(44.7971423090715,3.70657429374724,-10.0060406054345));
#6424=CARTESIAN_POINT('Ctrl Pts',(44.8208830494268,3.81057853813097,-9.94147707977391));
#6425=CARTESIAN_POINT('Ctrl Pts',(44.8208830494268,4.02761715699281,-9.85554541157574));
#6426=CARTESIAN_POINT('Ctrl Pts',(44.7971423090715,4.14762976290671,-9.83141439176083));
#6427=CARTESIAN_POINT('Ctrl Pts',(44.7111607127654,4.37771254887065,-9.82576392582316));
#6428=CARTESIAN_POINT('Ctrl Pts',(44.6493790253187,4.48794378495868,-9.84383347054759));
#6429=CARTESIAN_POINT('Ctrl Pts',(44.5419028922086,4.64227396980827,-9.89123304374228));
#6430=CARTESIAN_POINT('Ctrl Pts',(44.494558600482,4.7013640481238,-9.91589403100848));
#6431=CARTESIAN_POINT('Ctrl Pts',(44.4440437425414,4.7570246699791,-9.94551605816493));
#6432=CARTESIAN_POINT('',(65.0333054217745,3.34045249029966,-10.5063766605837));
#6433=CARTESIAN_POINT('Origin',(65.0333054217745,1.45964577074129,-11.5542860156157));
#6434=CARTESIAN_POINT('',(40.4874595913632,2.13422472611394,-10.8160833110905));
#6435=CARTESIAN_POINT('',(40.4874595913632,0.622676406422437,-11.0070362708084));
#6436=CARTESIAN_POINT('Ctrl Pts',(40.4874595913632,2.13422472611395,-10.8160833110905));
#6437=CARTESIAN_POINT('Ctrl Pts',(40.4362950734394,2.08749753761475,-10.7733834160453));
#6438=CARTESIAN_POINT('Ctrl Pts',(40.3883369165899,2.03616440970357,-10.7346520453388));
#6439=CARTESIAN_POINT('Ctrl Pts',(40.2799612282044,1.89833877684727,-10.6504382473029));
#6440=CARTESIAN_POINT('Ctrl Pts',(40.2177890646542,1.79624384746427,-10.6056498197694));
#6441=CARTESIAN_POINT('Ctrl Pts',(40.1312057824654,1.57225634809974,-10.5540221152286));
#6442=CARTESIAN_POINT('Ctrl Pts',(40.107260046221,1.45010114475192,-10.5475438114751));
#6443=CARTESIAN_POINT('Ctrl Pts',(40.107260046221,1.21852392960205,-10.5767988171273));
#6444=CARTESIAN_POINT('Ctrl Pts',(40.1312057824654,1.10181754522459,-10.6134523567928));
#6445=CARTESIAN_POINT('Ctrl Pts',(40.2177890646542,0.897706313053607,-10.719161508002));
#6446=CARTESIAN_POINT('Ctrl Pts',(40.2799612282044,0.809957312606231,-10.7879328011928));
#6447=CARTESIAN_POINT('Ctrl Pts',(40.3883369165899,0.697404845380977,-10.9037767089884));
#6448=CARTESIAN_POINT('Ctrl Pts',(40.4362950734394,0.657316542288901,-10.9540572922503));
#6449=CARTESIAN_POINT('Ctrl Pts',(40.4874595913632,0.622676406422431,-11.0070362708084));
#6450=CARTESIAN_POINT('',(44.4440437425414,2.13422472611394,-10.8160833110905));
#6451=CARTESIAN_POINT('',(65.0333054217745,2.13422472611395,-10.8160833110905));
#6452=CARTESIAN_POINT('',(44.4440437425414,0.622676406422437,-11.0070362708084));
#6453=CARTESIAN_POINT('Ctrl Pts',(44.4440437425414,0.622676406422432,-11.0070362708084));
#6454=CARTESIAN_POINT('Ctrl Pts',(44.494558600482,0.657181660752668,-10.9542635814532));
#6455=CARTESIAN_POINT('Ctrl Pts',(44.5419028922086,0.697082169882407,-10.9041861312438));
#6456=CARTESIAN_POINT('Ctrl Pts',(44.6493790253187,0.809487823261111,-10.788300435046));
#6457=CARTESIAN_POINT('Ctrl Pts',(44.7111607127654,0.897379122234209,-10.7193616693125));
#6458=CARTESIAN_POINT('Ctrl Pts',(44.7971423090715,1.10172433726337,-10.6134699828733));
#6459=CARTESIAN_POINT('Ctrl Pts',(44.8208830494268,1.21851739297085,-10.5767996428959));
#6460=CARTESIAN_POINT('Ctrl Pts',(44.8208830494268,1.45010768138313,-10.5475429857066));
#6461=CARTESIAN_POINT('Ctrl Pts',(44.7971423090715,1.57235101118944,-10.5540160076761));
#6462=CARTESIAN_POINT('Ctrl Pts',(44.7111607127654,1.79661053707614,-10.6057623235963));
#6463=CARTESIAN_POINT('Ctrl Pts',(44.6493790253187,1.89888494314277,-10.6506775740104));
#6464=CARTESIAN_POINT('Ctrl Pts',(44.5419028922086,2.0365787669325,-10.7349683587078));
#6465=CARTESIAN_POINT('Ctrl Pts',(44.494558600482,2.08767948363808,-10.7735496806195));
#6466=CARTESIAN_POINT('Ctrl Pts',(44.4440437425414,2.13422472611394,-10.8160833110905));
#6467=CARTESIAN_POINT('',(65.0333054217745,0.622676406422429,-11.0070362708084));
#6468=CARTESIAN_POINT('Origin',(65.0333054217745,-1.45964577074129,-11.5542860156157));
#6469=CARTESIAN_POINT('',(40.4874595913632,-0.622676406422435,-11.0070362708084));
#6470=CARTESIAN_POINT('',(40.4874595913632,-2.13422472611394,-10.8160833110905));
#6471=CARTESIAN_POINT('Ctrl Pts',(40.4874595913632,-0.62267640642243,-11.0070362708084));
#6472=CARTESIAN_POINT('Ctrl Pts',(40.4362950734394,-0.657316542288899,-10.9540572922503));
#6473=CARTESIAN_POINT('Ctrl Pts',(40.3883369165899,-0.697404845380975,-10.9037767089884));
#6474=CARTESIAN_POINT('Ctrl Pts',(40.2799612282044,-0.809957312606229,-10.7879328011928));
#6475=CARTESIAN_POINT('Ctrl Pts',(40.2177890646542,-0.897706313053603,-10.719161508002));
#6476=CARTESIAN_POINT('Ctrl Pts',(40.1312057824654,-1.10181754522459,-10.6134523567928));
#6477=CARTESIAN_POINT('Ctrl Pts',(40.107260046221,-1.21852392960205,-10.5767988171273));
#6478=CARTESIAN_POINT('Ctrl Pts',(40.107260046221,-1.45010114475192,-10.5475438114751));
#6479=CARTESIAN_POINT('Ctrl Pts',(40.1312057824654,-1.57225634809973,-10.5540221152286));
#6480=CARTESIAN_POINT('Ctrl Pts',(40.2177890646542,-1.79624384746427,-10.6056498197694));
#6481=CARTESIAN_POINT('Ctrl Pts',(40.2799612282044,-1.89833877684727,-10.6504382473029));
#6482=CARTESIAN_POINT('Ctrl Pts',(40.3883369165899,-2.03616440970357,-10.7346520453388));
#6483=CARTESIAN_POINT('Ctrl Pts',(40.4362950734394,-2.08749753761475,-10.7733834160453));
#6484=CARTESIAN_POINT('Ctrl Pts',(40.4874595913632,-2.13422472611394,-10.8160833110905));
#6485=CARTESIAN_POINT('',(44.4440437425414,-0.622676406422435,-11.0070362708084));
#6486=CARTESIAN_POINT('',(65.0333054217745,-0.622676406422428,-11.0070362708084));
#6487=CARTESIAN_POINT('',(44.4440437425414,-2.13422472611394,-10.8160833110905));
#6488=CARTESIAN_POINT('Ctrl Pts',(44.4440437425414,-2.13422472611394,-10.8160833110905));
#6489=CARTESIAN_POINT('Ctrl Pts',(44.494558600482,-2.08767948363808,-10.7735496806195));
#6490=CARTESIAN_POINT('Ctrl Pts',(44.5419028922086,-2.0365787669325,-10.7349683587078));
#6491=CARTESIAN_POINT('Ctrl Pts',(44.6493790253187,-1.89888494314277,-10.6506775740104));
#6492=CARTESIAN_POINT('Ctrl Pts',(44.7111607127654,-1.79661053707614,-10.6057623235963));
#6493=CARTESIAN_POINT('Ctrl Pts',(44.7971423090715,-1.57235101118944,-10.5540160076761));
#6494=CARTESIAN_POINT('Ctrl Pts',(44.8208830494268,-1.45010768138313,-10.5475429857066));
#6495=CARTESIAN_POINT('Ctrl Pts',(44.8208830494268,-1.21851739297084,-10.5767996428959));
#6496=CARTESIAN_POINT('Ctrl Pts',(44.7971423090715,-1.10172433726336,-10.6134699828733));
#6497=CARTESIAN_POINT('Ctrl Pts',(44.7111607127654,-0.897379122234208,-10.7193616693125));
#6498=CARTESIAN_POINT('Ctrl Pts',(44.6493790253187,-0.80948782326111,-10.788300435046));
#6499=CARTESIAN_POINT('Ctrl Pts',(44.5419028922086,-0.697082169882405,-10.9041861312438));
#6500=CARTESIAN_POINT('Ctrl Pts',(44.494558600482,-0.657181660752664,-10.9542635814532));
#6501=CARTESIAN_POINT('Ctrl Pts',(44.4440437425414,-0.62267640642243,-11.0070362708084));
#6502=CARTESIAN_POINT('',(65.0333054217745,-2.13422472611394,-10.8160833110905));
#6503=CARTESIAN_POINT('Origin',(65.0333054217745,-4.28722240024656,-10.8282877315631));
#6504=CARTESIAN_POINT('',(40.4874595913632,-3.34045249029966,-10.5063766605837));
#6505=CARTESIAN_POINT('',(40.4874595913632,-4.75702466997909,-9.94551605816494));
#6506=CARTESIAN_POINT('Ctrl Pts',(40.4874595913632,-3.34045249029965,-10.5063766605837));
#6507=CARTESIAN_POINT('Ctrl Pts',(40.4362950734394,-3.3608290063994,-10.4464474625785));
#6508=CARTESIAN_POINT('Ctrl Pts',(40.3883369165899,-3.38715358915463,-10.3877769807267));
#6509=CARTESIAN_POINT('Ctrl Pts',(40.2799612282044,-3.46736080529405,-10.2475818619421));
#6510=CARTESIAN_POINT('Ctrl Pts',(40.2177890646542,-3.53525028438945,-10.1591488563684));
#6511=CARTESIAN_POINT('Ctrl Pts',(40.1312057824654,-3.70666018998098,-10.0060003532323));
#6512=CARTESIAN_POINT('Ctrl Pts',(40.107260046221,-3.8105846640416,-9.94147465435432));
#6513=CARTESIAN_POINT('Ctrl Pts',(40.107260046221,-4.02761103108217,-9.85554783699534));
#6514=CARTESIAN_POINT('Ctrl Pts',(40.1312057824654,-4.14753959271859,-9.83144384918648));
#6515=CARTESIAN_POINT('Ctrl Pts',(40.2177890646542,-4.3773294009232,-9.82574614850904));
#6516=CARTESIAN_POINT('Ctrl Pts',(40.2799612282044,-4.4873552593498,-9.84373748876312));
#6517=CARTESIAN_POINT('Ctrl Pts',(40.3883369165899,-4.64179396643757,-9.89102971439187));
#6518=CARTESIAN_POINT('Ctrl Pts',(40.4362950734394,-4.70114646995115,-9.91577823807761));
#6519=CARTESIAN_POINT('Ctrl Pts',(40.4874595913632,-4.75702466997909,-9.94551605816493));
#6520=CARTESIAN_POINT('',(44.4440437425414,-3.34045249029966,-10.5063766605837));
#6521=CARTESIAN_POINT('',(65.0333054217745,-3.34045249029965,-10.5063766605837));
#6522=CARTESIAN_POINT('',(44.4440437425414,-4.75702466997909,-9.94551605816494));
#6523=CARTESIAN_POINT('Ctrl Pts',(44.4440437425414,-4.75702466997909,-9.94551605816493));
#6524=CARTESIAN_POINT('Ctrl Pts',(44.494558600482,-4.70136404812379,-9.91589403100848));
#6525=CARTESIAN_POINT('Ctrl Pts',(44.5419028922086,-4.64227396980827,-9.89123304374228));
#6526=CARTESIAN_POINT('Ctrl Pts',(44.6493790253187,-4.48794378495868,-9.84383347054759));
#6527=CARTESIAN_POINT('Ctrl Pts',(44.7111607127654,-4.37771254887065,-9.82576392582317));
#6528=CARTESIAN_POINT('Ctrl Pts',(44.7971423090715,-4.14762976290671,-9.83141439176083));
#6529=CARTESIAN_POINT('Ctrl Pts',(44.8208830494268,-4.02761715699281,-9.85554541157574));
#6530=CARTESIAN_POINT('Ctrl Pts',(44.8208830494268,-3.81057853813097,-9.94147707977391));
#6531=CARTESIAN_POINT('Ctrl Pts',(44.7971423090715,-3.70657429374724,-10.0060406054345));
#6532=CARTESIAN_POINT('Ctrl Pts',(44.7111607127654,-3.53498315096503,-10.1594240982912));
#6533=CARTESIAN_POINT('Ctrl Pts',(44.6493790253187,-3.46699749264153,-10.2480547031541));
#6534=CARTESIAN_POINT('Ctrl Pts',(44.5419028922086,-3.38694287027471,-10.3882537863625));
#6535=CARTESIAN_POINT('Ctrl Pts',(44.494558600482,-3.36074966445324,-10.4466808145008));
#6536=CARTESIAN_POINT('Ctrl Pts',(44.4440437425414,-3.34045249029965,-10.5063766605837));
#6537=CARTESIAN_POINT('',(65.0333054217745,-4.7570246699791,-9.94551605816494));
#6538=CARTESIAN_POINT('Origin',(65.0333054217745,-6.8454170790433,-9.42190830567978));
#6539=CARTESIAN_POINT('',(40.4874595913632,-5.84833565888647,-9.34556276502401));
#6540=CARTESIAN_POINT('',(40.4874595913632,-7.08092325871652,-8.45003545425543));
#6541=CARTESIAN_POINT('Ctrl Pts',(40.4874595913632,-5.84833565888646,-9.34556276502402));
#6542=CARTESIAN_POINT('Ctrl Pts',(40.4362950734394,-5.85316822377335,-9.28244891948659));
#6543=CARTESIAN_POINT('Ctrl Pts',(40.3883369165899,-5.86407501584219,-9.21907502119462));
#6544=CARTESIAN_POINT('Ctrl Pts',(40.2799612282044,-5.90689726652424,-9.06333766633591));
#6545=CARTESIAN_POINT('Ctrl Pts',(40.2177890646542,-5.95066147861605,-8.96079951935328));
#6546=CARTESIAN_POINT('Ctrl Pts',(40.1312057824654,-6.07859974285827,-8.76983454798312));
#6547=CARTESIAN_POINT('Ctrl Pts',(40.107260046221,-6.16321234968933,-8.68149107686204));
#6548=CARTESIAN_POINT('Ctrl Pts',(40.107260046221,-6.35205130381232,-8.54429154574763));
#6549=CARTESIAN_POINT('Ctrl Pts',(40.1312057824654,-6.46221767114332,-8.49111980857872));
#6550=CARTESIAN_POINT('Ctrl Pts',(40.2177890646542,-6.68337124943071,-8.42845471017137));
#6551=CARTESIAN_POINT('Ctrl Pts',(40.2799612282044,-6.79441470756917,-8.41851850107028));
#6552=CARTESIAN_POINT('Ctrl Pts',(40.3883369165899,-6.95576253693625,-8.42591760982703));
#6553=CARTESIAN_POINT('Ctrl Pts',(40.4362950734394,-7.01940507997324,-8.4351282457301));
#6554=CARTESIAN_POINT('Ctrl Pts',(40.4874595913632,-7.08092325871652,-8.45003545425542));
#6555=CARTESIAN_POINT('',(44.4440437425414,-5.84833565888647,-9.34556276502401));
#6556=CARTESIAN_POINT('',(65.0333054217745,-5.84833565888646,-9.34556276502402));
#6557=CARTESIAN_POINT('',(44.4440437425414,-7.08092325871652,-8.45003545425543));
#6558=CARTESIAN_POINT('Ctrl Pts',(44.4440437425414,-7.08092325871652,-8.45003545425542));
#6559=CARTESIAN_POINT('Ctrl Pts',(44.494558600482,-7.0196446190584,-8.43518629132191));
#6560=CARTESIAN_POINT('Ctrl Pts',(44.5419028922086,-6.9562780260716,-8.42599517922791));
#6561=CARTESIAN_POINT('Ctrl Pts',(44.6493790253187,-6.79500861326297,-8.41846510704323));
#6562=CARTESIAN_POINT('Ctrl Pts',(44.7111607127654,-6.68374678111907,-8.42837664395866));
#6563=CARTESIAN_POINT('Ctrl Pts',(44.7971423090715,-6.4622976827053,-8.49106885219836));
#6564=CARTESIAN_POINT('Ctrl Pts',(44.8208830494268,-6.35205663408888,-8.54428767307503));
#6565=CARTESIAN_POINT('Ctrl Pts',(44.8208830494268,-6.16320701941278,-8.68149494953464));
#6566=CARTESIAN_POINT('Ctrl Pts',(44.7971423090715,-6.07852655552829,-8.76989489711301));
#6567=CARTESIAN_POINT('Ctrl Pts',(44.7111607127654,-5.95047118756212,-8.96113254742615));
#6568=CARTESIAN_POINT('Ctrl Pts',(44.6493790253187,-5.90666295883444,-9.06388600455431));
#6569=CARTESIAN_POINT('Ctrl Pts',(44.5419028922086,-5.86398949382312,-9.21958925075898));
#6570=CARTESIAN_POINT('Ctrl Pts',(44.494558600482,-5.85314940676355,-9.28269467176876));
#6571=CARTESIAN_POINT('Ctrl Pts',(44.4440437425414,-5.84833565888646,-9.34556276502402));
#6572=CARTESIAN_POINT('',(65.0333054217745,-7.08092325871653,-8.45003545425542));
#6573=CARTESIAN_POINT('Origin',(65.0333054217745,-8.97348902708079,-7.42351572959578));
#6574=CARTESIAN_POINT('',(40.4874595913632,-7.98874638935144,-7.59753279036232));
#6575=CARTESIAN_POINT('',(40.4874595913632,-8.9599013972947,-6.42360804569852));
#6576=CARTESIAN_POINT('Ctrl Pts',(40.4874595913632,-7.98874638935143,-7.59753279036232));
#6577=CARTESIAN_POINT('Ctrl Pts',(40.4362950734394,-7.97773135520069,-7.53519997232426));
#6578=CARTESIAN_POINT('Ctrl Pts',(40.3883369165899,-7.97253504272507,-7.47110467269465));
#6579=CARTESIAN_POINT('Ctrl Pts',(40.2799612282044,-7.97528164845017,-7.30961063252953));
#6580=CARTESIAN_POINT('Ctrl Pts',(40.2177890646542,-7.99217072713915,-7.19941019302185));
#6581=CARTESIAN_POINT('Ctrl Pts',(40.1312057824654,-8.06859851836571,-6.98262778488883));
#6582=CARTESIAN_POINT('Ctrl Pts',(40.107260046221,-8.12858273669663,-6.87601748671976));
#6583=CARTESIAN_POINT('Ctrl Pts',(40.107260046221,-8.27736883191338,-6.69616599297443));
#6584=CARTESIAN_POINT('Ctrl Pts',(40.1312057824654,-8.370850846916,-6.61726748224376));
#6585=CARTESIAN_POINT('Ctrl Pts',(40.2177890646542,-8.56947230261641,-6.50157246470553));
#6586=CARTESIAN_POINT('Ctrl Pts',(40.2799612282044,-8.67455609160262,-6.46433303480991));
#6587=CARTESIAN_POINT('Ctrl Pts',(40.3883369165899,-8.83267496573407,-6.43137411347947));
#6588=CARTESIAN_POINT('Ctrl Pts',(40.4362950734394,-8.89660865325455,-6.42446812347171));
#6589=CARTESIAN_POINT('Ctrl Pts',(40.4874595913632,-8.9599013972947,-6.42360804569852));
#6590=CARTESIAN_POINT('',(44.4440437425414,-7.98874638935144,-7.59753279036232));
#6591=CARTESIAN_POINT('',(65.0333054217745,-7.98874638935143,-7.59753279036232));
#6592=CARTESIAN_POINT('',(44.4440437425414,-8.9599013972947,-6.42360804569852));
#6593=CARTESIAN_POINT('Ctrl Pts',(44.4440437425414,-8.9599013972947,-6.42360804569852));
#6594=CARTESIAN_POINT('Ctrl Pts',(44.494558600482,-8.89685510213054,-6.42446477450646));
#6595=CARTESIAN_POINT('Ctrl Pts',(44.5419028922086,-8.83319355055587,-6.43132104896007));
#6596=CARTESIAN_POINT('Ctrl Pts',(44.6493790253187,-8.67511806010238,-6.46413361991443));
#6597=CARTESIAN_POINT('Ctrl Pts',(44.7111607127654,-8.5698166220086,-6.50140346015324));
#6598=CARTESIAN_POINT('Ctrl Pts',(44.7971423090715,-8.37091567243115,-6.61719822868546));
#6599=CARTESIAN_POINT('Ctrl Pts',(44.8208830494268,-8.27737303163499,-6.69616091638308));
#6600=CARTESIAN_POINT('Ctrl Pts',(44.8208830494268,-8.12857853697502,-6.87602256331111));
#6601=CARTESIAN_POINT('Ctrl Pts',(44.7971423090715,-8.06854263856858,-6.98270443898868));
#6602=CARTESIAN_POINT('Ctrl Pts',(44.7111607127654,-7.99206923514248,-7.19978008186616));
#6603=CARTESIAN_POINT('Ctrl Pts',(44.6493790253187,-7.97519106813697,-7.31020001364741));
#6604=CARTESIAN_POINT('Ctrl Pts',(44.5419028922086,-7.97258009122984,-7.47162401525293));
#6605=CARTESIAN_POINT('Ctrl Pts',(44.494558600482,-7.97777424546919,-7.53544268344662));
#6606=CARTESIAN_POINT('Ctrl Pts',(44.4440437425414,-7.98874638935143,-7.59753279036232));
#6607=CARTESIAN_POINT('',(65.0333054217745,-8.9599013972947,-6.42360804569852));
#6608=CARTESIAN_POINT('Origin',(65.0333054217745,-10.5377236573627,-4.95867635844022));
#6609=CARTESIAN_POINT('',(40.4874595913632,-9.62719480361945,-5.37212188871111));
#6610=CARTESIAN_POINT('',(40.4874595913632,-10.2758959788686,-3.99356171925254));
#6611=CARTESIAN_POINT('Ctrl Pts',(40.4874595913632,-9.62719480361944,-5.37212188871112));
#6612=CARTESIAN_POINT('Ctrl Pts',(40.4362950734394,-9.60102428553722,-5.31448669837382));
#6613=CARTESIAN_POINT('Ctrl Pts',(40.3883369165899,-9.58005137194069,-5.25369734080832));
#6614=CARTESIAN_POINT('Ctrl Pts',(40.2799612282044,-9.54254975336982,-5.0965938798139));
#6615=CARTESIAN_POINT('Ctrl Pts',(40.2177890646542,-9.53150249572826,-4.9856554466843));
#6616=CARTESIAN_POINT('Ctrl Pts',(40.1312057824654,-9.55161757473464,-4.75667683776135));
#6617=CARTESIAN_POINT('Ctrl Pts',(40.107260046221,-9.58320437552114,-4.6384984296635));
#6618=CARTESIAN_POINT('Ctrl Pts',(40.107260046221,-9.68258883427221,-4.42729570408679));
#6619=CARTESIAN_POINT('Ctrl Pts',(40.1312057824654,-9.75351267814104,-4.32762790339198));
#6620=CARTESIAN_POINT('Ctrl Pts',(40.2177890646542,-9.9171218947142,-4.16617251017132));
#6621=CARTESIAN_POINT('Ctrl Pts',(40.2799612282044,-10.009643213615,-4.10396974981856));
#6622=CARTESIAN_POINT('Ctrl Pts',(40.3883369165899,-10.1545979421286,-4.03272372864255));
#6623=CARTESIAN_POINT('Ctrl Pts',(40.4362950734393,-10.214805585414,-4.01013504147461));
#6624=CARTESIAN_POINT('Ctrl Pts',(40.4874595913632,-10.2758959788686,-3.99356171925254));
#6625=CARTESIAN_POINT('',(44.4440437425414,-9.62719480361945,-5.37212188871111));
#6626=CARTESIAN_POINT('',(65.0333054217745,-9.62719480361944,-5.37212188871112));
#6627=CARTESIAN_POINT('',(44.4440437425414,-10.2758959788686,-3.99356171925254));
#6628=CARTESIAN_POINT('Ctrl Pts',(44.4440437425414,-10.2758959788686,-3.99356171925254));
#6629=CARTESIAN_POINT('Ctrl Pts',(44.494558600482,-10.2150434587916,-4.0100705083801));
#6630=CARTESIAN_POINT('Ctrl Pts',(44.5419028922086,-10.1550870380453,-4.03254336444179));
#6631=CARTESIAN_POINT('Ctrl Pts',(44.6493790253187,-10.0101379343731,-4.10363684402592));
#6632=CARTESIAN_POINT('Ctrl Pts',(44.7111607127654,-9.91741336695648,-4.16592318645703));
#6633=CARTESIAN_POINT('Ctrl Pts',(44.7971423090715,-9.75355824438383,-4.32754470411152));
#6634=CARTESIAN_POINT('Ctrl Pts',(44.8208830494268,-9.68259163955491,-4.4272897425576));
#6635=CARTESIAN_POINT('Ctrl Pts',(44.8208830494268,-9.58320157023844,-4.63850439119269));
#6636=CARTESIAN_POINT('Ctrl Pts',(44.7971423090715,-9.55158251360353,-4.75676498037214));
#6637=CARTESIAN_POINT('Ctrl Pts',(44.7111607127654,-9.53149617990424,-4.98603895482358));
#6638=CARTESIAN_POINT('Ctrl Pts',(44.6493790253187,-9.54260859192742,-5.09718727084803));
#6639=CARTESIAN_POINT('Ctrl Pts',(44.5419028922086,-9.58022416040605,-5.25418916415756));
#6640=CARTESIAN_POINT('Ctrl Pts',(44.494558600482,-9.60112618813069,-5.31471111790393));
#6641=CARTESIAN_POINT('Ctrl Pts',(44.4440437425414,-9.62719480361944,-5.37212188871112));
#6642=CARTESIAN_POINT('',(65.0333054217745,-10.2758959788686,-3.99356171925253));
#6643=CARTESIAN_POINT('Origin',(65.0333054217745,-11.4398343552159,-2.18226511494789));
#6644=CARTESIAN_POINT('',(40.4874595913632,-10.6607311620303,-2.80916081150993));
#6645=CARTESIAN_POINT('',(40.4874595913632,-10.9462182239883,-1.31258522269331));
#6646=CARTESIAN_POINT('Ctrl Pts',(40.4874595913632,-10.6607311620303,-2.80916081150993));
#6647=CARTESIAN_POINT('Ctrl Pts',(40.4362950734394,-10.6210495499161,-2.7598446798497));
#6648=CARTESIAN_POINT('Ctrl Pts',(40.3883369165899,-10.5856178404929,-2.70618088325177));
#6649=CARTESIAN_POINT('Ctrl Pts',(40.2799612282044,-10.5102243622422,-2.56333938966843));
#6650=CARTESIAN_POINT('Ctrl Pts',(40.2177890646542,-10.4719349080967,-2.45863363267347));
#6651=CARTESIAN_POINT('Ctrl Pts',(40.1312057824654,-10.4344733704908,-2.23184639108363));
#6652=CARTESIAN_POINT('Ctrl Pts',(40.107260046221,-10.4356780388714,-2.10952545706757));
#6653=CARTESIAN_POINT('Ctrl Pts',(40.107260046221,-10.479416170103,-1.88024214365675));
#6654=CARTESIAN_POINT('Ctrl Pts',(40.1312057824654,-10.5233254368881,-1.76606754746801));
#6655=CARTESIAN_POINT('Ctrl Pts',(40.2177890646542,-10.6416422455441,-1.56899661471236));
#6656=CARTESIAN_POINT('Ctrl Pts',(40.2799612282044,-10.7157876396233,-1.48573895210117));
#6657=CARTESIAN_POINT('Ctrl Pts',(40.3883369165899,-10.8384701838204,-1.38068248061461));
#6658=CARTESIAN_POINT('Ctrl Pts',(40.4362950734394,-10.8911687152148,-1.34383042657664));
#6659=CARTESIAN_POINT('Ctrl Pts',(40.4874595913632,-10.9462182239883,-1.31258522269331));
#6660=CARTESIAN_POINT('',(44.4440437425414,-10.6607311620303,-2.80916081150993));
#6661=CARTESIAN_POINT('',(65.0333054217746,-10.6607311620303,-2.80916081150993));
#6662=CARTESIAN_POINT('',(44.4440437425414,-10.9462182239883,-1.31258522269331));
#6663=CARTESIAN_POINT('Ctrl Pts',(44.4440437425414,-10.9462182239883,-1.31258522269331));
#6664=CARTESIAN_POINT('Ctrl Pts',(44.494558600482,-10.8913830666349,-1.34370876420452));
#6665=CARTESIAN_POINT('Ctrl Pts',(44.5419028922086,-10.8388990591367,-1.38038614967856));
#6666=CARTESIAN_POINT('Ctrl Pts',(44.6493790253187,-10.7161840275151,-1.48529347310667));
#6667=CARTESIAN_POINT('Ctrl Pts',(44.7111607127654,-10.6418625563635,-1.56868263776198));
#6668=CARTESIAN_POINT('Ctrl Pts',(44.7971423090715,-10.5233488807639,-1.76597563018215));
#6669=CARTESIAN_POINT('Ctrl Pts',(44.8208830494268,-10.4794174046805,-1.88023567177453));
#6670=CARTESIAN_POINT('Ctrl Pts',(44.8208830494268,-10.4356768042938,-2.10953192894979));
#6671=CARTESIAN_POINT('Ctrl Pts',(44.7971423090715,-10.4344613310455,-2.23194048388096));
#6672=CARTESIAN_POINT('Ctrl Pts',(44.7111607127654,-10.4720241652918,-2.45900666288089));
#6673=CARTESIAN_POINT('Ctrl Pts',(44.6493790253187,-10.5104289226276,-2.5638995056778));
#6674=CARTESIAN_POINT('Ctrl Pts',(44.5419028922086,-10.5859075119841,-2.70661428432213));
#6675=CARTESIAN_POINT('Ctrl Pts',(44.494558600482,-10.6212040619198,-2.76003670668311));
#6676=CARTESIAN_POINT('Ctrl Pts',(44.4440437425414,-10.6607311620303,-2.80916081150993));
#6677=CARTESIAN_POINT('',(65.0333054217746,-10.9462182239883,-1.31258522269331));
#6678=CARTESIAN_POINT('Origin',(65.0333054217745,-11.6231381877631,0.731265871526303));
#6679=CARTESIAN_POINT('',(40.4874595913632,-11.0244145741041,-0.0696898291507972));
#6680=CARTESIAN_POINT('',(40.4874595913632,-10.9287493207203,1.45086583075851));
#6681=CARTESIAN_POINT('Ctrl Pts',(40.4874595913632,-11.0244145741041,-0.0696898291508038));
#6682=CARTESIAN_POINT('Ctrl Pts',(40.4362950734394,-10.9737152095859,-0.031791470091884));
#6683=CARTESIAN_POINT('Ctrl Pts',(40.3883369165899,-10.9260510089478,0.0113748718365901));
#6684=CARTESIAN_POINT('Ctrl Pts',(40.2799612282044,-10.8175029205336,0.130979141632737));
#6685=CARTESIAN_POINT('Ctrl Pts',(40.2177890646542,-10.7543771371068,0.222873174700234));
#6686=CARTESIAN_POINT('Ctrl Pts',(40.1312057824654,-10.6616928290704,0.433219172502735));
#6687=CARTESIAN_POINT('Ctrl Pts',(40.107260046221,-10.6324396713002,0.551996758287847));
#6688=CARTESIAN_POINT('Ctrl Pts',(40.107260046221,-10.6177832473694,0.784953945706132));
#6689=CARTESIAN_POINT('Ctrl Pts',(40.1312057824654,-10.6319189563517,0.906461327605488));
#6690=CARTESIAN_POINT('Ctrl Pts',(40.2177890646542,-10.6975090768639,1.12676510841489));
#6691=CARTESIAN_POINT('Ctrl Pts',(40.2799612282044,-10.7486197183239,1.22584628814239));
#6692=CARTESIAN_POINT('Ctrl Pts',(40.3883369165899,-10.8413214827577,1.35811212546531));
#6693=CARTESIAN_POINT('Ctrl Pts',(40.4362950734394,-10.8831996597221,1.40691199628575));
#6694=CARTESIAN_POINT('Ctrl Pts',(40.4874595913632,-10.9287493207203,1.45086583075852));
#6695=CARTESIAN_POINT('',(44.4440437425414,-11.0244145741041,-0.0696898291507972));
#6696=CARTESIAN_POINT('',(65.0333054217745,-11.0244145741041,-0.0696898291508069));
#6697=CARTESIAN_POINT('',(44.4440437425414,-10.9287493207203,1.45086583075851));
#6698=CARTESIAN_POINT('Ctrl Pts',(44.4440437425414,-10.9287493207203,1.45086583075852));
#6699=CARTESIAN_POINT('Ctrl Pts',(44.494558600482,-10.8833770206965,1.40708314344117));
#6700=CARTESIAN_POINT('Ctrl Pts',(44.5419028922086,-10.8416631896602,1.35850580357412));
#6701=CARTESIAN_POINT('Ctrl Pts',(44.6493790253187,-10.7488928668403,1.22637634925516));
#6702=CARTESIAN_POINT('Ctrl Pts',(44.7111607127654,-10.6976443833215,1.12712401027483));
#6703=CARTESIAN_POINT('Ctrl Pts',(44.7971423090715,-10.6319188047956,0.906556187395612));
#6704=CARTESIAN_POINT('Ctrl Pts',(44.8208830494268,-10.6177828336688,0.78496052128923));
#6705=CARTESIAN_POINT('Ctrl Pts',(44.8208830494268,-10.6324400850008,0.551990182704752));
#6706=CARTESIAN_POINT('Ctrl Pts',(44.7971423090715,-10.6617045677936,0.433125041715377));
#6707=CARTESIAN_POINT('Ctrl Pts',(44.7111607127654,-10.7545563589632,0.222534061284506));
#6708=CARTESIAN_POINT('Ctrl Pts',(44.6493790253187,-10.8178403494655,0.130487494796954));
#6709=CARTESIAN_POINT('Ctrl Pts',(44.5419028922086,-10.9264393623398,0.0110271252282851));
#6710=CARTESIAN_POINT('Ctrl Pts',(44.494558600482,-10.9739126224425,-0.0319390384764412));
#6711=CARTESIAN_POINT('Ctrl Pts',(44.4440437425414,-11.0244145741041,-0.0696898291508038));
#6712=CARTESIAN_POINT('',(65.0333054217745,-10.9287493207203,1.45086583075852));
#6713=CARTESIAN_POINT('Origin',(65.0333054217745,-11.0761175010611,3.59884873388475));
#6714=CARTESIAN_POINT('',(40.4874595913632,-10.6953934735264,2.67416002147514));
#6715=CARTESIAN_POINT('',(40.4874595913632,-10.2245869045029,4.1231536481525));
#6716=CARTESIAN_POINT('Ctrl Pts',(40.4874595913632,-10.6953934735264,2.67416002147514));
#6717=CARTESIAN_POINT('Ctrl Pts',(40.4362950734394,-10.636861984136,2.69825931465265));
#6718=CARTESIAN_POINT('Ctrl Pts',(40.3883369165899,-10.5799602093058,2.7282159018936));
#6719=CARTESIAN_POINT('Ctrl Pts',(40.2799612282044,-10.445077986335,2.81706777175753));
#6720=CARTESIAN_POINT('Ctrl Pts',(40.2177890646542,-10.3610822987601,2.89037604083732));
#6721=CARTESIAN_POINT('Ctrl Pts',(40.1312057824654,-10.2189989162361,3.07106398221209));
#6722=CARTESIAN_POINT('Ctrl Pts',(40.107260046221,-10.1611260158034,3.17883498721797));
#6723=CARTESIAN_POINT('Ctrl Pts',(40.107260046221,-10.0889959537284,3.40082849180162));
#6724=CARTESIAN_POINT('Ctrl Pts',(40.1312057824654,-10.072469906325,3.52203390373397));
#6725=CARTESIAN_POINT('Ctrl Pts',(40.2177890646542,-10.0812120701981,3.75172803582824));
#6726=CARTESIAN_POINT('Ctrl Pts',(40.2799612282044,-10.1060764894642,3.86040709775467));
#6727=CARTESIAN_POINT('Ctrl Pts',(40.3883369165899,-10.162972681342,4.01157155191524));
#6728=CARTESIAN_POINT('Ctrl Pts',(40.4362950734394,-10.1913991440005,4.06925296416112));
#6729=CARTESIAN_POINT('Ctrl Pts',(40.4874595913632,-10.2245869045029,4.12315364815251));
#6730=CARTESIAN_POINT('',(44.4440437425414,-10.6953934735264,2.67416002147514));
#6731=CARTESIAN_POINT('',(65.0333054217745,-10.6953934735264,2.67416002147513));
#6732=CARTESIAN_POINT('',(44.4440437425414,-10.2245869045029,4.1231536481525));
#6733=CARTESIAN_POINT('Ctrl Pts',(44.4440437425414,-10.2245869045029,4.12315364815251));
#6734=CARTESIAN_POINT('Ctrl Pts',(44.494558600482,-10.191528370287,4.06946284229464));
#6735=CARTESIAN_POINT('Ctrl Pts',(44.5419028922086,-10.1632057491294,4.01203784095338));
#6736=CARTESIAN_POINT('Ctrl Pts',(44.6493790253187,-10.1062092356792,3.86098843529658));
#6737=CARTESIAN_POINT('Ctrl Pts',(44.7111607127654,-10.0812538704914,3.75210931147394));
#6738=CARTESIAN_POINT('Ctrl Pts',(44.7971423090715,-10.0724461688598,3.52212574563888));
#6739=CARTESIAN_POINT('Ctrl Pts',(44.8208830494268,-10.088993917744,3.40083475791753));
#6740=CARTESIAN_POINT('Ctrl Pts',(44.8208830494268,-10.1611280517879,3.17882872110207));
#6741=CARTESIAN_POINT('Ctrl Pts',(44.7971423090715,-10.2190336955406,3.07097572801825));
#6742=CARTESIAN_POINT('Ctrl Pts',(44.7111607127654,-10.3613402241094,2.89009215195637));
#6743=CARTESIAN_POINT('Ctrl Pts',(44.6493790253187,-10.4455270819127,2.81667548607418));
#6744=CARTESIAN_POINT('Ctrl Pts',(44.5419028922086,-10.5804228429266,2.72797565994568));
#6745=CARTESIAN_POINT('Ctrl Pts',(44.494558600482,-10.6370898936696,2.69816547698127));
#6746=CARTESIAN_POINT('Ctrl Pts',(44.4440437425414,-10.6953934735264,2.67416002147514));
#6747=CARTESIAN_POINT('',(65.0333054217745,-10.2245869045029,4.12315364815251));
#6748=CARTESIAN_POINT('Origin',(65.0333054217745,-9.83314361665672,6.24030269465341));
#6749=CARTESIAN_POINT('',(40.4874595913632,-9.69434146610128,5.2499825630792));
#6750=CARTESIAN_POINT('',(40.4874595913632,-8.87797608967546,6.53636855793469));
#6751=CARTESIAN_POINT('Ctrl Pts',(40.4874595913632,-9.69434146610128,5.24998256307919));
#6752=CARTESIAN_POINT('Ctrl Pts',(40.4362950734394,-9.63165560058094,5.25876854315396));
#6753=CARTESIAN_POINT('Ctrl Pts',(40.3883369165899,-9.56909159934126,5.27363309315841));
#6754=CARTESIAN_POINT('Ctrl Pts',(40.2799612282044,-9.4163503879453,5.32614967333225));
#6755=CARTESIAN_POINT('Ctrl Pts',(40.2177890646542,-9.31676255418716,5.3762659502691));
#6756=CARTESIAN_POINT('Ctrl Pts',(40.1312057824654,-9.13420771864564,5.51594254733579));
#6757=CARTESIAN_POINT('Ctrl Pts',(40.107260046221,-9.05135144272633,5.6059353229639));
#6758=CARTESIAN_POINT('Ctrl Pts',(40.107260046221,-8.92627993958308,5.80301647638493));
#6759=CARTESIAN_POINT('Ctrl Pts',(40.1312057824654,-8.88013052813091,5.91630413655623));
#6760=CARTESIAN_POINT('Ctrl Pts',(40.2177890646542,-8.83147543305722,6.14095609285995));
#6761=CARTESIAN_POINT('Ctrl Pts',(40.2799612282044,-8.82853130722192,6.25240433183085));
#6762=CARTESIAN_POINT('Ctrl Pts',(40.3883369165899,-8.8460469295586,6.41296918423019));
#6763=CARTESIAN_POINT('Ctrl Pts',(40.4362950734394,-8.85923553871714,6.4759078026327));
#6764=CARTESIAN_POINT('Ctrl Pts',(40.4874595913632,-8.87797608967545,6.53636855793469));
#6765=CARTESIAN_POINT('',(44.4440437425414,-9.69434146610128,5.2499825630792));
#6766=CARTESIAN_POINT('',(65.0333054217745,-9.69434146610129,5.24998256307919));
#6767=CARTESIAN_POINT('',(44.4440437425414,-8.87797608967546,6.53636855793469));
#6768=CARTESIAN_POINT('Ctrl Pts',(44.4440437425414,-8.87797608967545,6.53636855793469));
#6769=CARTESIAN_POINT('Ctrl Pts',(44.494558600482,-8.85930851055284,6.47614322432933));
#6770=CARTESIAN_POINT('Ctrl Pts',(44.5419028922086,-8.8461567137246,6.4134787855425));
#6771=CARTESIAN_POINT('Ctrl Pts',(44.6493790253187,-8.82851531020285,6.25300041822613));
#6772=CARTESIAN_POINT('Ctrl Pts',(44.7111607127654,-8.83142110072016,6.14133578534036));
#6773=CARTESIAN_POINT('Ctrl Pts',(44.7971423090715,-8.88008469626887,5.91638718981127));
#6774=CARTESIAN_POINT('Ctrl Pts',(44.8208830494268,-8.92627640924315,5.80302203931053));
#6775=CARTESIAN_POINT('Ctrl Pts',(44.8208830494268,-9.05135497306626,5.6059297600383));
#6776=CARTESIAN_POINT('Ctrl Pts',(44.7971423090715,-9.13426335321985,5.51586571507106));
#6777=CARTESIAN_POINT('Ctrl Pts',(44.7111607127654,-9.31708297663107,5.37605512370539));
#6778=CARTESIAN_POINT('Ctrl Pts',(44.6493790253187,-9.41688293184191,5.32588139755355));
#6779=CARTESIAN_POINT('Ctrl Pts',(44.5419028922086,-9.56959944421904,5.27351545115601));
#6780=CARTESIAN_POINT('Ctrl Pts',(44.494558600482,-9.6318996863973,5.25873433236176));
#6781=CARTESIAN_POINT('Ctrl Pts',(44.4440437425414,-9.69434146610128,5.24998256307919));
#6782=CARTESIAN_POINT('',(65.0333054217745,-8.87797608967545,6.5363685579347));
#6783=CARTESIAN_POINT('Origin',(65.0333054217745,-7.97231715504529,8.48965548688909));
#6784=CARTESIAN_POINT('',(40.4874595913632,-8.08415833106712,7.49592939215974));
#6785=CARTESIAN_POINT('',(40.4874595913632,-6.97352938622158,8.53887939213984));
#6786=CARTESIAN_POINT('Ctrl Pts',(40.4874595913632,-8.08415833106713,7.49592939215973));
#6787=CARTESIAN_POINT('Ctrl Pts',(40.4362950734394,-8.02125687288993,7.48885000369108));
#6788=CARTESIAN_POINT('Ctrl Pts',(40.3883369165899,-7.95696177153298,7.48768852211428));
#6789=CARTESIAN_POINT('Ctrl Pts',(40.2799612282044,-7.79595886376674,7.50057000272323));
#6790=CARTESIAN_POINT('Ctrl Pts',(40.2177890646542,-7.68703635367879,7.52434529752241));
#6791=CARTESIAN_POINT('Ctrl Pts',(40.1312057824654,-7.47548065682658,7.61423415599275));
#6792=CARTESIAN_POINT('Ctrl Pts',(40.107260046221,-7.3728471699607,7.68079412518008));
#6793=CARTESIAN_POINT('Ctrl Pts',(40.107260046221,-7.20269292827251,7.84057959375527));
#6794=CARTESIAN_POINT('Ctrl Pts',(40.1312057824654,-7.12981989001877,7.93883122183408));
#6795=CARTESIAN_POINT('Ctrl Pts',(40.2177890646542,-7.02682471456273,8.14432529372061));
#6796=CARTESIAN_POINT('Ctrl Pts',(40.2799612282044,-6.99625703388003,8.25154000700348));
#6797=CARTESIAN_POINT('Ctrl Pts',(40.3883369165899,-6.97329151570619,8.41141637744911));
#6798=CARTESIAN_POINT('Ctrl Pts',(40.4362950734394,-6.97041358254702,8.47565753714199));
#6799=CARTESIAN_POINT('Ctrl Pts',(40.4874595913632,-6.97352938622157,8.53887939213984));
#6800=CARTESIAN_POINT('',(44.4440437425414,-8.08415833106712,7.49592939215974));
#6801=CARTESIAN_POINT('',(65.0333054217745,-8.08415833106713,7.49592939215973));
#6802=CARTESIAN_POINT('',(44.4440437425414,-6.97352938622158,8.53887939213984));
#6803=CARTESIAN_POINT('Ctrl Pts',(44.4440437425414,-6.97352938622157,8.53887939213984));
#6804=CARTESIAN_POINT('Ctrl Pts',(44.494558600482,-6.97042571484315,8.47590370999069));
#6805=CARTESIAN_POINT('Ctrl Pts',(44.5419028922086,-6.97327111810788,8.41193727091097));
#6806=CARTESIAN_POINT('Ctrl Pts',(44.6493790253187,-6.99609329877835,8.25211338795166));
#6807=CARTESIAN_POINT('Ctrl Pts',(44.7111607127654,-7.02667766349585,8.14467954556077));
#6808=CARTESIAN_POINT('Ctrl Pts',(44.7971423090715,-7.12975484354433,7.9389002678978));
#6809=CARTESIAN_POINT('Ctrl Pts',(44.8208830494268,-7.20268812540135,7.84058410395149));
#6810=CARTESIAN_POINT('Ctrl Pts',(44.8208830494268,-7.37285197283185,7.68078961498386));
#6811=CARTESIAN_POINT('Ctrl Pts',(44.7971423090715,-7.47555365094558,7.61417357331087));
#6812=CARTESIAN_POINT('Ctrl Pts',(44.7111607127654,-7.68739913989675,7.5242207802843));
#6813=CARTESIAN_POINT('Ctrl Pts',(44.6493790253187,-7.79654139429069,7.500442593603));
#6814=CARTESIAN_POINT('Ctrl Pts',(44.5419028922086,-7.95748291790636,7.48770087193706));
#6815=CARTESIAN_POINT('Ctrl Pts',(44.494558600482,-8.02150179817958,7.48887756936796));
#6816=CARTESIAN_POINT('Ctrl Pts',(44.4440437425414,-8.08415833106713,7.49592939215973));
#6817=CARTESIAN_POINT('',(65.0333054217745,-6.97352938622157,8.53887939213985));
#6818=CARTESIAN_POINT('Origin',(65.0333054217745,-5.61056068645084,10.2055720021147));
#6819=CARTESIAN_POINT('',(40.4874595913632,-5.96601779663743,9.270879409431));
#6820=CARTESIAN_POINT('',(40.4874595913632,-4.63091018458434,10.0048610303352));
#6821=CARTESIAN_POINT('Ctrl Pts',(40.4874595913632,-5.96601779663743,9.270879409431));
#6822=CARTESIAN_POINT('Ctrl Pts',(40.4362950734394,-5.90685307575603,9.24837947643258));
#6823=CARTESIAN_POINT('Ctrl Pts',(40.3883369165899,-5.84486677196091,9.23126494343361));
#6824=CARTESIAN_POINT('Ctrl Pts',(40.2799612282044,-5.68571857264663,9.20370193367626));
#6825=CARTESIAN_POINT('Ctrl Pts',(40.2177890646542,-5.57430538812665,9.19964235712612));
#6826=CARTESIAN_POINT('Ctrl Pts',(40.1312057824654,-5.3470416524444,9.2340954294343));
#6827=CARTESIAN_POINT('Ctrl Pts',(40.107260046221,-5.2310797940713,9.27304038452639));
#6828=CARTESIAN_POINT('Ctrl Pts',(40.107260046221,-5.02653423062696,9.3854902596153));
#6829=CARTESIAN_POINT('Ctrl Pts',(40.1312057824654,-4.93151644657342,9.46253234446524));
#6830=CARTESIAN_POINT('Ctrl Pts',(40.2177890646542,-4.78065275639871,9.63595658364359));
#6831=CARTESIAN_POINT('Ctrl Pts',(40.2799612282044,-4.72438220066596,9.73220107649475));
#6832=CARTESIAN_POINT('Ctrl Pts',(40.3883369165899,-4.66237854994973,9.88134334464741));
#6833=CARTESIAN_POINT('Ctrl Pts',(40.4362950734394,-4.64361490559755,9.94285053730468));
#6834=CARTESIAN_POINT('Ctrl Pts',(40.4874595913632,-4.63091018458433,10.0048610303352));
#6835=CARTESIAN_POINT('',(44.4440437425414,-5.96601779663743,9.270879409431));
#6836=CARTESIAN_POINT('',(65.0333054217745,-5.96601779663744,9.270879409431));
#6837=CARTESIAN_POINT('',(44.4440437425414,-4.63091018458434,10.0048610303352));
#6838=CARTESIAN_POINT('Ctrl Pts',(44.4440437425414,-4.63091018458433,10.0048610303352));
#6839=CARTESIAN_POINT('Ctrl Pts',(44.494558600482,-4.64356543603732,9.94309199336002));
#6840=CARTESIAN_POINT('Ctrl Pts',(44.5419028922086,-4.66222925224323,9.88184280060688));
#6841=CARTESIAN_POINT('Ctrl Pts',(44.6493790253187,-4.72408101556028,9.7327157243621));
#6842=CARTESIAN_POINT('Ctrl Pts',(44.7111607127654,-4.78042222636134,9.63626313589754));
#6843=CARTESIAN_POINT('Ctrl Pts',(44.7971423090715,-4.93143627259579,9.4625830449195));
#6844=CARTESIAN_POINT('Ctrl Pts',(44.8208830494268,-5.02652845700664,9.38549343368993));
#6845=CARTESIAN_POINT('Ctrl Pts',(44.8208830494268,-5.23108556769161,9.27303721045176));
#6846=CARTESIAN_POINT('Ctrl Pts',(44.7971423090715,-5.34712741961925,9.23405490296801));
#6847=CARTESIAN_POINT('Ctrl Pts',(44.7111607127654,-5.57468774292635,9.19961197308963));
#6848=CARTESIAN_POINT('Ctrl Pts',(44.6493790253187,-5.6863144872627,9.20372339679809));
#6849=CARTESIAN_POINT('Ctrl Pts',(44.5419028922086,-5.84536847428662,9.2314065090968));
#6850=CARTESIAN_POINT('Ctrl Pts',(44.494558600482,-5.90708345096224,9.24846708652567));
#6851=CARTESIAN_POINT('Ctrl Pts',(44.4440437425414,-5.96601779663743,9.270879409431));
#6852=CARTESIAN_POINT('',(65.0333054217745,-4.63091018458433,10.0048610303352));
#6853=CARTESIAN_POINT('Origin',(65.0333054217745,-2.89627205572787,11.2802348949791));
#6854=CARTESIAN_POINT('',(40.4874595913632,-3.47301042256638,10.4633059774983));
#6855=CARTESIAN_POINT('',(40.4874595913632,-1.99731386475336,10.8422004546895));
#6856=CARTESIAN_POINT('Ctrl Pts',(40.4874595913632,-3.47301042256639,10.4633059774983));
#6857=CARTESIAN_POINT('Ctrl Pts',(40.4362950734394,-3.42129997598637,10.4267992535094));
#6858=CARTESIAN_POINT('Ctrl Pts',(40.3883369165899,-3.36551729719021,10.3948070381394));
#6859=CARTESIAN_POINT('Ctrl Pts',(40.2799612282044,-3.21822367299693,10.3285314232885));
#6860=CARTESIAN_POINT('Ctrl Pts',(40.2177890646542,-3.11132031417736,10.2968920535137));
#6861=CARTESIAN_POINT('Ctrl Pts',(40.1312057824654,-2.88262835599554,10.2737445264171));
#6862=CARTESIAN_POINT('Ctrl Pts',(40.107260046221,-2.76062443615468,10.282627412656));
#6863=CARTESIAN_POINT('Ctrl Pts',(40.107260046221,-2.53453990097136,10.3406760550451));
#6864=CARTESIAN_POINT('Ctrl Pts',(40.1312057824654,-2.42334768794107,10.391667759134));
#6865=CARTESIAN_POINT('Ctrl Pts',(40.2177890646542,-2.23409480353921,10.5221252828469));
#6866=CARTESIAN_POINT('Ctrl Pts',(40.2799612282044,-2.15565705872172,10.601352159818));
#6867=CARTESIAN_POINT('Ctrl Pts',(40.3883369165899,-2.05851119287108,10.7303891684628));
#6868=CARTESIAN_POINT('Ctrl Pts',(40.4362950734394,-2.02504082610839,10.7852976709622));
#6869=CARTESIAN_POINT('Ctrl Pts',(40.4874595913632,-1.99731386475336,10.8422004546895));
#6870=CARTESIAN_POINT('',(44.4440437425414,-3.47301042256638,10.4633059774983));
#6871=CARTESIAN_POINT('',(65.0333054217745,-3.47301042256639,10.4633059774983));
#6872=CARTESIAN_POINT('',(44.4440437425414,-1.99731386475336,10.8422004546895));
#6873=CARTESIAN_POINT('Ctrl Pts',(44.4440437425414,-1.99731386475336,10.8422004546895));
#6874=CARTESIAN_POINT('Ctrl Pts',(44.494558600482,-2.0249328630462,10.7855192386522));
#6875=CARTESIAN_POINT('Ctrl Pts',(44.5419028922086,-2.05824237598036,10.7308358042651));
#6876=CARTESIAN_POINT('Ctrl Pts',(44.6493790253187,-2.15523734817991,10.6017757373863));
#6877=CARTESIAN_POINT('Ctrl Pts',(44.7111607127654,-2.23379527958143,10.5223648737091));
#6878=CARTESIAN_POINT('Ctrl Pts',(44.7971423090715,-2.42325742408613,10.3916969282828));
#6879=CARTESIAN_POINT('Ctrl Pts',(44.8208830494268,-2.53453351937968,10.3406776935593));
#6880=CARTESIAN_POINT('Ctrl Pts',(44.8208830494268,-2.76063081774636,10.2826257741417));
#6881=CARTESIAN_POINT('Ctrl Pts',(44.7971423090715,-2.8827215071592,10.2737266025933));
#6882=CARTESIAN_POINT('Ctrl Pts',(44.7111607127654,-3.11169821280053,10.2969577118196));
#6883=CARTESIAN_POINT('Ctrl Pts',(44.6493790253187,-3.21879552819819,10.3287004100455));
#6884=CARTESIAN_POINT('Ctrl Pts',(44.5419028922086,-3.36596803166599,10.3950689245517));
#6885=CARTESIAN_POINT('Ctrl Pts',(44.494558600482,-3.42150132578769,10.4269414031543));
#6886=CARTESIAN_POINT('Ctrl Pts',(44.4440437425414,-3.47301042256638,10.4633059774983));
#6887=CARTESIAN_POINT('',(65.0333054217745,-1.99731386475336,10.8422004546896));
#6888=CARTESIAN_POINT('Origin',(45.2000998321956,0.,0.));
#6889=CARTESIAN_POINT('',(45.9561559218497,-1.16412425803185E-15,9.50579594738959));
#6890=CARTESIAN_POINT('Origin',(45.9561559218497,0.,0.));
#6891=CARTESIAN_POINT('',(44.8208830494268,-4.43719969509731E-16,10.6461191435901));
#6892=CARTESIAN_POINT('',(45.2000998321956,-1.25712631749648E-15,10.265215394118));
#6893=CARTESIAN_POINT('',(44.4440437425414,-0.761781030806626,10.9982845496518));
#6894=CARTESIAN_POINT('Ctrl Pts',(44.8208830494268,4.5102810375397E-16,
10.6461191435901));
#6895=CARTESIAN_POINT('Ctrl Pts',(44.8208830494268,-0.11671548063215,10.6461191435901));
#6896=CARTESIAN_POINT('Ctrl Pts',(44.7971423090715,-0.237183600496259,10.6678622756543));
#6897=CARTESIAN_POINT('Ctrl Pts',(44.7111607127654,-0.45318923993895,10.7473077279545));
#6898=CARTESIAN_POINT('Ctrl Pts',(44.6493790253187,-0.549027808195105,10.8046871902268));
#6899=CARTESIAN_POINT('Ctrl Pts',(44.5419028922086,-0.675071438451299,10.9055709290878));
#6900=CARTESIAN_POINT('Ctrl Pts',(44.494558600482,-0.720933688912239,10.9502526438148));
#6901=CARTESIAN_POINT('Ctrl Pts',(44.4440437425414,-0.761781030806632,10.9982845496518));
#6902=CARTESIAN_POINT('Origin',(44.4440437425414,0.,0.));
#6903=CARTESIAN_POINT('Origin',(44.4440437425414,0.,0.));
#6904=CARTESIAN_POINT('Origin',(44.4440437425414,0.,0.));
#6905=CARTESIAN_POINT('Origin',(44.4440437425414,0.,0.));
#6906=CARTESIAN_POINT('Origin',(44.4440437425414,0.,0.));
#6907=CARTESIAN_POINT('Origin',(44.4440437425414,0.,0.));
#6908=CARTESIAN_POINT('Origin',(44.4440437425414,0.,0.));
#6909=CARTESIAN_POINT('Origin',(44.4440437425414,0.,0.));
#6910=CARTESIAN_POINT('Origin',(44.4440437425414,0.,0.));
#6911=CARTESIAN_POINT('Origin',(44.4440437425414,0.,0.));
#6912=CARTESIAN_POINT('Origin',(44.4440437425414,0.,0.));
#6913=CARTESIAN_POINT('Origin',(44.4440437425414,0.,0.));
#6914=CARTESIAN_POINT('Origin',(44.4440437425414,0.,0.));
#6915=CARTESIAN_POINT('Origin',(44.4440437425414,0.,0.));
#6916=CARTESIAN_POINT('Origin',(44.4440437425414,0.,0.));
#6917=CARTESIAN_POINT('Origin',(44.4440437425414,0.,0.));
#6918=CARTESIAN_POINT('Origin',(44.4440437425414,0.,0.));
#6919=CARTESIAN_POINT('Origin',(44.4440437425414,0.,0.));
#6920=CARTESIAN_POINT('Origin',(44.4440437425414,0.,0.));
#6921=CARTESIAN_POINT('Origin',(44.4440437425414,0.,0.));
#6922=CARTESIAN_POINT('Origin',(44.4440437425414,0.,0.));
#6923=CARTESIAN_POINT('Origin',(44.4440437425414,0.,0.));
#6924=CARTESIAN_POINT('Origin',(44.4440437425414,0.,0.));
#6925=CARTESIAN_POINT('Origin',(44.4440437425414,0.,0.));
#6926=CARTESIAN_POINT('',(44.4440437425414,0.761781030806626,10.9982845496518));
#6927=CARTESIAN_POINT('Origin',(44.4440437425414,0.,0.));
#6928=CARTESIAN_POINT('Ctrl Pts',(44.4440437425414,0.761781030806632,10.9982845496518));
#6929=CARTESIAN_POINT('Ctrl Pts',(44.494558600482,0.720933688912238,10.9502526438148));
#6930=CARTESIAN_POINT('Ctrl Pts',(44.5419028922086,0.6750714384513,10.9055709290878));
#6931=CARTESIAN_POINT('Ctrl Pts',(44.6493790253187,0.549027808195106,10.8046871902268));
#6932=CARTESIAN_POINT('Ctrl Pts',(44.7111607127654,0.45318923993895,10.7473077279545));
#6933=CARTESIAN_POINT('Ctrl Pts',(44.7971423090715,0.23718360049626,10.6678622756543));
#6934=CARTESIAN_POINT('Ctrl Pts',(44.8208830494268,0.116715480632151,10.6461191435901));
#6935=CARTESIAN_POINT('Ctrl Pts',(44.8208830494268,3.46944695195361E-17,
10.6461191435901));
#6936=CARTESIAN_POINT('Origin',(42.4657516669523,0.,0.));
#6937=CARTESIAN_POINT('',(40.4874595913632,0.761781030806626,10.9982845496518));
#6938=CARTESIAN_POINT('Origin',(40.4874595913632,0.,0.));
#6939=CARTESIAN_POINT('',(65.0333054217745,0.761781030806634,10.9982845496518));
#6940=CARTESIAN_POINT('Origin',(42.4657516669523,0.,0.));
#6941=CARTESIAN_POINT('',(40.4874595913632,-0.761781030806626,10.9982845496518));
#6942=CARTESIAN_POINT('',(65.0333054217745,-0.761781030806634,10.9982845496518));
#6943=CARTESIAN_POINT('Origin',(40.4874595913632,0.,0.));
#6944=CARTESIAN_POINT('Origin',(42.4657516669523,0.,0.));
#6945=CARTESIAN_POINT('Origin',(40.4874595913632,0.,0.));
#6946=CARTESIAN_POINT('Origin',(42.4657516669523,0.,0.));
#6947=CARTESIAN_POINT('Origin',(40.4874595913632,0.,0.));
#6948=CARTESIAN_POINT('Origin',(42.4657516669523,0.,0.));
#6949=CARTESIAN_POINT('Origin',(40.4874595913632,0.,0.));
#6950=CARTESIAN_POINT('Origin',(42.4657516669523,0.,0.));
#6951=CARTESIAN_POINT('Origin',(40.4874595913632,0.,0.));
#6952=CARTESIAN_POINT('Origin',(42.4657516669523,0.,0.));
#6953=CARTESIAN_POINT('Origin',(40.4874595913632,0.,0.));
#6954=CARTESIAN_POINT('Origin',(42.4657516669523,0.,0.));
#6955=CARTESIAN_POINT('Origin',(40.4874595913632,0.,0.));
#6956=CARTESIAN_POINT('Origin',(42.4657516669523,0.,0.));
#6957=CARTESIAN_POINT('Origin',(40.4874595913632,0.,0.));
#6958=CARTESIAN_POINT('Origin',(42.4657516669523,0.,0.));
#6959=CARTESIAN_POINT('Origin',(40.4874595913632,0.,0.));
#6960=CARTESIAN_POINT('Origin',(42.4657516669523,0.,0.));
#6961=CARTESIAN_POINT('Origin',(40.4874595913632,0.,0.));
#6962=CARTESIAN_POINT('Origin',(42.4657516669523,0.,0.));
#6963=CARTESIAN_POINT('Origin',(40.4874595913632,0.,0.));
#6964=CARTESIAN_POINT('Origin',(42.4657516669523,0.,0.));
#6965=CARTESIAN_POINT('Origin',(40.4874595913632,0.,0.));
#6966=CARTESIAN_POINT('Origin',(42.4657516669523,0.,0.));
#6967=CARTESIAN_POINT('Origin',(40.4874595913632,0.,0.));
#6968=CARTESIAN_POINT('Origin',(42.4657516669523,0.,0.));
#6969=CARTESIAN_POINT('Origin',(40.4874595913632,0.,0.));
#6970=CARTESIAN_POINT('Origin',(42.4657516669523,0.,0.));
#6971=CARTESIAN_POINT('Origin',(40.4874595913632,0.,0.));
#6972=CARTESIAN_POINT('Origin',(42.4657516669523,0.,0.));
#6973=CARTESIAN_POINT('Origin',(40.4874595913632,0.,0.));
#6974=CARTESIAN_POINT('Origin',(42.4657516669523,0.,0.));
#6975=CARTESIAN_POINT('Origin',(40.4874595913632,0.,0.));
#6976=CARTESIAN_POINT('Origin',(42.4657516669523,0.,0.));
#6977=CARTESIAN_POINT('Origin',(40.4874595913632,0.,0.));
#6978=CARTESIAN_POINT('Origin',(42.4657516669523,0.,0.));
#6979=CARTESIAN_POINT('Origin',(40.4874595913632,0.,0.));
#6980=CARTESIAN_POINT('Origin',(42.4657516669523,0.,0.));
#6981=CARTESIAN_POINT('Origin',(40.4874595913632,0.,0.));
#6982=CARTESIAN_POINT('Origin',(42.4657516669523,0.,0.));
#6983=CARTESIAN_POINT('Origin',(40.4874595913632,0.,0.));
#6984=CARTESIAN_POINT('Origin',(42.4657516669523,0.,0.));
#6985=CARTESIAN_POINT('Origin',(40.4874595913632,0.,0.));
#6986=CARTESIAN_POINT('Origin',(42.4657516669523,0.,0.));
#6987=CARTESIAN_POINT('Origin',(40.4874595913632,0.,0.));
#6988=CARTESIAN_POINT('Origin',(65.0333054217745,0.,11.6461191435901));
#6989=CARTESIAN_POINT('',(40.107260046221,-7.55970195185556E-16,10.6461191435901));
#6990=CARTESIAN_POINT('Ctrl Pts',(40.4874595913632,-0.761781030806633,10.9982845496518));
#6991=CARTESIAN_POINT('Ctrl Pts',(40.4362950734394,-0.720774016064355,10.9500648864029));
#6992=CARTESIAN_POINT('Ctrl Pts',(40.3883369165899,-0.674699993130249,10.9052051772128));
#6993=CARTESIAN_POINT('Ctrl Pts',(40.2799612282044,-0.548515944174103,10.804381297894));
#6994=CARTESIAN_POINT('Ctrl Pts',(40.2177890646542,-0.452839542252609,10.7471501528591));
#6995=CARTESIAN_POINT('Ctrl Pts',(40.1312057824654,-0.237088918373978,10.6678564706158));
#6996=CARTESIAN_POINT('Ctrl Pts',(40.107260046221,-0.116708892047988,10.6461191435901));
#6997=CARTESIAN_POINT('Ctrl Pts',(40.107260046221,-1.56125112837913E-16,
10.6461191435901));
#6998=CARTESIAN_POINT('Ctrl Pts',(40.107260046221,1.73472347597681E-17,
10.6461191435901));
#6999=CARTESIAN_POINT('Ctrl Pts',(40.107260046221,0.116708892047988,10.6461191435901));
#7000=CARTESIAN_POINT('Ctrl Pts',(40.1312057824654,0.237088918373978,10.6678564706158));
#7001=CARTESIAN_POINT('Ctrl Pts',(40.2177890646542,0.452839542252609,10.7471501528591));
#7002=CARTESIAN_POINT('Ctrl Pts',(40.2799612282044,0.548515944174103,10.804381297894));
#7003=CARTESIAN_POINT('Ctrl Pts',(40.3883369165899,0.674699993130249,10.9052051772128));
#7004=CARTESIAN_POINT('Ctrl Pts',(40.4362950734394,0.720774016064356,10.9500648864029));
#7005=CARTESIAN_POINT('Ctrl Pts',(40.4874595913632,0.761781030806633,10.9982845496518));
#7006=CARTESIAN_POINT('Origin',(51.9780076285768,0.,0.));
#7007=CARTESIAN_POINT('',(52.9998593353039,-1.16412425803185E-15,9.50579594738959));
#7008=CARTESIAN_POINT('Origin',(52.9998593353039,0.,0.));
#7009=CARTESIAN_POINT('',(51.9780076285768,-1.16412425803185E-15,9.50579594738959));
#7010=CARTESIAN_POINT('Origin',(52.9998593353039,0.,0.));
#7011=CARTESIAN_POINT('Origin',(21.2197085942866,0.,-9.50579594738959));
#7012=CARTESIAN_POINT('',(21.2197085942866,-1.16412425803185E-15,9.50579594738959));
#7013=CARTESIAN_POINT('Origin',(21.2197085942866,0.,0.));
#7014=CARTESIAN_POINT('Origin',(30.0907863269434,0.,0.));
#7015=CARTESIAN_POINT('',(38.9618640596001,-1.16412425803185E-15,9.50579594738959));
#7016=CARTESIAN_POINT('Origin',(38.9618640596001,0.,0.));
#7017=CARTESIAN_POINT('',(30.0907863269434,-1.16412425803185E-15,9.50579594738959));
#7018=CARTESIAN_POINT('Origin',(39.7246618254816,0.,0.));
#7019=CARTESIAN_POINT('Origin',(40.4874595913632,0.,0.));
#7020=CARTESIAN_POINT('',(39.7246618254816,-1.25712631749648E-15,10.265215394118));
#7021=CARTESIAN_POINT('Origin',(42.4657516669523,0.,0.));
#7022=CARTESIAN_POINT('',(0.,0.,0.));
#7023=CARTESIAN_POINT('Origin',(21.2197085942866,0.,0.));
#7024=CARTESIAN_POINT('',(30.0128737835214,9.5056654627527,-6.92688080986705E-16));
#7025=CARTESIAN_POINT('',(30.0129125498419,-1.16410452817968E-15,9.50563484084649));
#7026=CARTESIAN_POINT('Origin',(30.0129125498419,0.,0.));
#7027=CARTESIAN_POINT('Origin',(30.0129125498419,0.,0.));
#7028=CARTESIAN_POINT('',(14.0227085942866,9.50563484084649,-5.82052264084792E-16));
#7029=CARTESIAN_POINT('',(21.2197085942866,9.50579594738959,-1.16412425803185E-15));
#7030=CARTESIAN_POINT('',(14.0227085942866,1.16410452817062E-15,9.50563484084649));
#7031=CARTESIAN_POINT('Origin',(14.0227085942866,0.,0.));
#7032=CARTESIAN_POINT('Origin',(14.0227085942866,0.,0.));
#7033=CARTESIAN_POINT('',(27.1076139360583,-1.,9.45305012117298));
#7034=CARTESIAN_POINT('',(16.509210476167,-1.,9.45305012117298));
#7035=CARTESIAN_POINT('',(21.2197085942866,-1.,9.45305012117298));
#7036=CARTESIAN_POINT('',(27.1076139360583,1.,9.45305012117298));
#7037=CARTESIAN_POINT('Ctrl Pts',(27.1076139360583,1.,9.45305012117297));
#7038=CARTESIAN_POINT('Ctrl Pts',(27.2332762619206,1.,9.45305012117297));
#7039=CARTESIAN_POINT('Ctrl Pts',(27.3672506399949,0.974867302313412,9.45581410516793));
#7040=CARTESIAN_POINT('Ctrl Pts',(27.6136022144272,0.872784825785775,9.46578223306855));
#7041=CARTESIAN_POINT('Ctrl Pts',(27.7259873812924,0.795840117138944,9.47284078387221));
#7042=CARTESIAN_POINT('Ctrl Pts',(27.9034536829199,0.618373815511396,9.48607862959468));
#7043=CARTESIAN_POINT('Ctrl Pts',(27.9803986808371,0.505988486616992,9.49312009999403));
#7044=CARTESIAN_POINT('Ctrl Pts',(28.0824813722535,0.259636368087859,9.50304911791651));
#7045=CARTESIAN_POINT('Ctrl Pts',(28.1076139360583,0.125661801483354,9.50579594738959));
#7046=CARTESIAN_POINT('Ctrl Pts',(28.1076139360583,-0.125661801483354,9.5057959473896));
#7047=CARTESIAN_POINT('Ctrl Pts',(28.0824813722535,-0.259636368087854,9.50304911791651));
#7048=CARTESIAN_POINT('Ctrl Pts',(27.9803986808371,-0.505988486616989,9.49312009999403));
#7049=CARTESIAN_POINT('Ctrl Pts',(27.9034536829199,-0.618373815511396,9.48607862959468));
#7050=CARTESIAN_POINT('Ctrl Pts',(27.7259873812924,-0.795840117138944,9.47284078387221));
#7051=CARTESIAN_POINT('Ctrl Pts',(27.6136022144272,-0.872784825785776,9.46578223306855));
#7052=CARTESIAN_POINT('Ctrl Pts',(27.3672506399949,-0.974867302313412,9.45581410516794));
#7053=CARTESIAN_POINT('Ctrl Pts',(27.2332762619206,-1.,9.45305012117297));
#7054=CARTESIAN_POINT('Ctrl Pts',(27.1076139360583,-1.,9.45305012117297));
#7055=CARTESIAN_POINT('',(16.509210476167,1.,9.45305012117298));
#7056=CARTESIAN_POINT('',(21.2197085942866,1.,9.45305012117298));
#7057=CARTESIAN_POINT('Ctrl Pts',(16.509210476167,-1.,9.45305012117298));
#7058=CARTESIAN_POINT('Ctrl Pts',(16.3835481503047,-1.,9.45305012117298));
#7059=CARTESIAN_POINT('Ctrl Pts',(16.2495737722304,-0.974867302313413,9.45581410516794));
#7060=CARTESIAN_POINT('Ctrl Pts',(16.0032221977981,-0.872784825785775,9.46578223306855));
#7061=CARTESIAN_POINT('Ctrl Pts',(15.8908370309329,-0.795840117138944,9.47284078387221));
#7062=CARTESIAN_POINT('Ctrl Pts',(15.7133707293053,-0.618373815511396,9.48607862959468));
#7063=CARTESIAN_POINT('Ctrl Pts',(15.6364257313882,-0.505988486616992,9.49312009999403));
#7064=CARTESIAN_POINT('Ctrl Pts',(15.5343430399718,-0.259636368087859,9.50304911791651));
#7065=CARTESIAN_POINT('Ctrl Pts',(15.509210476167,-0.125661801483353,9.50579594738959));
#7066=CARTESIAN_POINT('Ctrl Pts',(15.509210476167,0.125661801483353,9.50579594738959));
#7067=CARTESIAN_POINT('Ctrl Pts',(15.5343430399718,0.259636368087859,9.50304911791651));
#7068=CARTESIAN_POINT('Ctrl Pts',(15.6364257313882,0.505988486616992,9.49312009999403));
#7069=CARTESIAN_POINT('Ctrl Pts',(15.7133707293053,0.618373815511395,9.48607862959468));
#7070=CARTESIAN_POINT('Ctrl Pts',(15.8908370309329,0.795840117138943,9.47284078387221));
#7071=CARTESIAN_POINT('Ctrl Pts',(16.0032221977981,0.872784825785773,9.46578223306855));
#7072=CARTESIAN_POINT('Ctrl Pts',(16.2495737722303,0.974867302313412,9.45581410516794));
#7073=CARTESIAN_POINT('Ctrl Pts',(16.3835481503047,1.,9.45305012117297));
#7074=CARTESIAN_POINT('Ctrl Pts',(16.509210476167,1.,9.45305012117297));
#7075=CARTESIAN_POINT('Origin',(27.1076139360583,1.,0.));
#7076=CARTESIAN_POINT('',(27.1076139360583,1.,10.9791881928495));
#7077=CARTESIAN_POINT('',(27.1076139360583,1.,0.));
#7078=CARTESIAN_POINT('',(16.509210476167,1.,10.9791881928495));
#7079=CARTESIAN_POINT('',(20.0171174336818,1.,10.9791881928495));
#7080=CARTESIAN_POINT('',(16.509210476167,1.,0.));
#7081=CARTESIAN_POINT('Origin',(27.1076139360583,0.,0.));
#7082=CARTESIAN_POINT('',(27.1076139360583,-1.,10.9791881928495));
#7083=CARTESIAN_POINT('',(27.1076139360583,-1.,0.));
#7084=CARTESIAN_POINT('',(28.1076139360583,-6.9241142324032E-16,11.0246348408465));
#7085=CARTESIAN_POINT('Ctrl Pts',(28.1076139360583,-1.38777878078145E-16,
11.0246348408465));
#7086=CARTESIAN_POINT('Ctrl Pts',(28.1076139360583,-0.125636205005722,11.0246348408465));
#7087=CARTESIAN_POINT('Ctrl Pts',(28.0824913810873,-0.259599701677183,11.0222671389354));
#7088=CARTESIAN_POINT('Ctrl Pts',(27.9804161707035,-0.505958788131831,11.0137083033886));
#7089=CARTESIAN_POINT('Ctrl Pts',(27.9034673289024,-0.618360169528907,11.00763882809));
#7090=CARTESIAN_POINT('Ctrl Pts',(27.7259739014455,-0.795853596985864,10.9962311251393));
#7091=CARTESIAN_POINT('Ctrl Pts',(27.6135726098982,-0.872802279941483,10.9901507178533));
#7092=CARTESIAN_POINT('Ctrl Pts',(27.3672138227875,-0.974877370414414,10.9815668619283));
#7093=CARTESIAN_POINT('Ctrl Pts',(27.2332504300619,-1.,10.9791881928495));
#7094=CARTESIAN_POINT('Ctrl Pts',(27.1076139360583,-1.,10.9791881928495));
#7095=CARTESIAN_POINT('Ctrl Pts',(27.1076139360583,1.,10.9791881928495));
#7096=CARTESIAN_POINT('Ctrl Pts',(27.2332504300619,1.,10.9791881928495));
#7097=CARTESIAN_POINT('Ctrl Pts',(27.3672138227875,0.974877370414413,10.9815668619283));
#7098=CARTESIAN_POINT('Ctrl Pts',(27.6135726098982,0.87280227994148,10.9901507178533));
#7099=CARTESIAN_POINT('Ctrl Pts',(27.7259739014455,0.795853596985865,10.9962311251393));
#7100=CARTESIAN_POINT('Ctrl Pts',(27.9034673289024,0.618360169528908,11.00763882809));
#7101=CARTESIAN_POINT('Ctrl Pts',(27.9804161707035,0.505958788131831,11.0137083033886));
#7102=CARTESIAN_POINT('Ctrl Pts',(28.0824913810873,0.259599701677183,11.0222671389354));
#7103=CARTESIAN_POINT('Ctrl Pts',(28.1076139360583,0.125636205005722,11.0246348408465));
#7104=CARTESIAN_POINT('Ctrl Pts',(28.1076139360583,-6.93889390390723E-17,
11.0246348408465));
#7105=CARTESIAN_POINT('Origin',(12.8302991238869,0.,12.));
#7106=CARTESIAN_POINT('',(12.8302991238869,1.,10.9791881928495));
#7107=CARTESIAN_POINT('',(13.8302991238869,-5.70980779921944E-16,11.0246348408465));
#7108=CARTESIAN_POINT('Ctrl Pts',(12.8302991238869,1.,10.9791881928495));
#7109=CARTESIAN_POINT('Ctrl Pts',(12.9559356178906,1.,10.9791881928495));
#7110=CARTESIAN_POINT('Ctrl Pts',(13.0898990106162,0.974877370414413,10.9815668619283));
#7111=CARTESIAN_POINT('Ctrl Pts',(13.3362577977268,0.87280227994148,10.9901507178533));
#7112=CARTESIAN_POINT('Ctrl Pts',(13.4486590892742,0.795853596985866,10.9962311251393));
#7113=CARTESIAN_POINT('Ctrl Pts',(13.6261525167311,0.618360169528908,11.00763882809));
#7114=CARTESIAN_POINT('Ctrl Pts',(13.7031013585322,0.505958788131832,11.0137083033886));
#7115=CARTESIAN_POINT('Ctrl Pts',(13.805176568916,0.259599701677187,11.0222671389354));
#7116=CARTESIAN_POINT('Ctrl Pts',(13.8302991238869,0.125636205005722,11.0246348408465));
#7117=CARTESIAN_POINT('Ctrl Pts',(13.8302991238869,-3.46944695195361E-17,
11.0246348408465));
#7118=CARTESIAN_POINT('',(11.8302991238869,1.22464679914735E-16,11.0246348408465));
#7119=CARTESIAN_POINT('Ctrl Pts',(11.8302991238869,-1.38777878078145E-16,
11.0246348408465));
#7120=CARTESIAN_POINT('Ctrl Pts',(11.8302991238869,0.125636205005722,11.0246348408465));
#7121=CARTESIAN_POINT('Ctrl Pts',(11.8554216788579,0.259599701677188,11.0222671389354));
#7122=CARTESIAN_POINT('Ctrl Pts',(11.9574968892417,0.505958788131833,11.0137083033886));
#7123=CARTESIAN_POINT('Ctrl Pts',(12.0344457310427,0.618360169528908,11.00763882809));
#7124=CARTESIAN_POINT('Ctrl Pts',(12.2119391584997,0.795853596985866,10.9962311251393));
#7125=CARTESIAN_POINT('Ctrl Pts',(12.324340450047,0.87280227994148,10.9901507178533));
#7126=CARTESIAN_POINT('Ctrl Pts',(12.5706992371577,0.974877370414413,10.9815668619283));
#7127=CARTESIAN_POINT('Ctrl Pts',(12.7046626298833,1.,10.9791881928495));
#7128=CARTESIAN_POINT('Ctrl Pts',(12.8302991238869,1.,10.9791881928495));
#7129=CARTESIAN_POINT('',(11.8302991238869,-1.22464679914735E-16,10.));
#7130=CARTESIAN_POINT('',(11.8302991238869,1.22464679914735E-16,12.));
#7131=CARTESIAN_POINT('Origin',(12.8302991238869,0.,10.));
#7132=CARTESIAN_POINT('Ctrl Pts',(13.8302991238869,2.77555756156289E-16,
11.0246348408465));
#7133=CARTESIAN_POINT('Ctrl Pts',(13.8302991238869,-0.125636205005722,11.0246348408465));
#7134=CARTESIAN_POINT('Ctrl Pts',(13.805176568916,-0.259599701677187,11.0222671389354));
#7135=CARTESIAN_POINT('Ctrl Pts',(13.7031013585322,-0.505958788131832,11.0137083033886));
#7136=CARTESIAN_POINT('Ctrl Pts',(13.6261525167311,-0.618360169528908,11.00763882809));
#7137=CARTESIAN_POINT('Ctrl Pts',(13.4486590892742,-0.795853596985866,10.9962311251393));
#7138=CARTESIAN_POINT('Ctrl Pts',(13.3362577977268,-0.87280227994148,10.9901507178533));
#7139=CARTESIAN_POINT('Ctrl Pts',(13.0898990106162,-0.974877370414413,10.9815668619283));
#7140=CARTESIAN_POINT('Ctrl Pts',(12.9559356178906,-1.,10.9791881928495));
#7141=CARTESIAN_POINT('Ctrl Pts',(12.7046626298833,-1.,10.9791881928495));
#7142=CARTESIAN_POINT('Ctrl Pts',(12.5706992371577,-0.974877370414413,10.9815668619283));
#7143=CARTESIAN_POINT('Ctrl Pts',(12.324340450047,-0.87280227994148,10.9901507178533));
#7144=CARTESIAN_POINT('Ctrl Pts',(12.2119391584997,-0.795853596985866,10.9962311251393));
#7145=CARTESIAN_POINT('Ctrl Pts',(12.0344457310427,-0.618360169528909,11.00763882809));
#7146=CARTESIAN_POINT('Ctrl Pts',(11.9574968892417,-0.505958788131833,11.0137083033886));
#7147=CARTESIAN_POINT('Ctrl Pts',(11.8554216788579,-0.259599701677187,11.0222671389354));
#7148=CARTESIAN_POINT('Ctrl Pts',(11.8302991238869,-0.125636205005722,11.0246348408465));
#7149=CARTESIAN_POINT('Ctrl Pts',(11.8302991238869,-6.93889390390723E-17,
11.0246348408465));
#7150=CARTESIAN_POINT('Origin',(12.8302991238869,0.,10.));
#7151=CARTESIAN_POINT('Origin',(16.509210476167,-1.,0.));
#7152=CARTESIAN_POINT('',(16.509210476167,-1.,10.9791881928495));
#7153=CARTESIAN_POINT('',(16.509210476167,-1.,0.));
#7154=CARTESIAN_POINT('',(20.0171174336818,-1.,10.9791881928495));
#7155=CARTESIAN_POINT('Origin',(16.509210476167,0.,0.));
#7156=CARTESIAN_POINT('',(15.509210476167,-7.79147597039161E-16,11.0246348408465));
#7157=CARTESIAN_POINT('Ctrl Pts',(15.509210476167,-1.73472347597681E-16,
11.0246348408465));
#7158=CARTESIAN_POINT('Ctrl Pts',(15.509210476167,0.125636205005722,11.0246348408465));
#7159=CARTESIAN_POINT('Ctrl Pts',(15.534333031138,0.259599701677186,11.0222671389354));
#7160=CARTESIAN_POINT('Ctrl Pts',(15.6364082415218,0.505958788131832,11.0137083033886));
#7161=CARTESIAN_POINT('Ctrl Pts',(15.7133570833229,0.618360169528908,11.00763882809));
#7162=CARTESIAN_POINT('Ctrl Pts',(15.8908505107798,0.795853596985865,10.9962311251393));
#7163=CARTESIAN_POINT('Ctrl Pts',(16.0032518023271,0.87280227994148,10.9901507178533));
#7164=CARTESIAN_POINT('Ctrl Pts',(16.2496105894378,0.974877370414413,10.9815668619283));
#7165=CARTESIAN_POINT('Ctrl Pts',(16.3835739821634,1.,10.9791881928495));
#7166=CARTESIAN_POINT('Ctrl Pts',(16.509210476167,1.,10.9791881928495));
#7167=CARTESIAN_POINT('Ctrl Pts',(16.509210476167,-1.,10.9791881928495));
#7168=CARTESIAN_POINT('Ctrl Pts',(16.3835739821634,-1.,10.9791881928495));
#7169=CARTESIAN_POINT('Ctrl Pts',(16.2496105894378,-0.974877370414412,10.9815668619283));
#7170=CARTESIAN_POINT('Ctrl Pts',(16.0032518023271,-0.872802279941479,10.9901507178533));
#7171=CARTESIAN_POINT('Ctrl Pts',(15.8908505107798,-0.795853596985865,10.9962311251393));
#7172=CARTESIAN_POINT('Ctrl Pts',(15.7133570833228,-0.618360169528908,11.00763882809));
#7173=CARTESIAN_POINT('Ctrl Pts',(15.6364082415218,-0.505958788131831,11.0137083033886));
#7174=CARTESIAN_POINT('Ctrl Pts',(15.534333031138,-0.259599701677186,11.0222671389354));
#7175=CARTESIAN_POINT('Ctrl Pts',(15.509210476167,-0.125636205005722,11.0246348408465));
#7176=CARTESIAN_POINT('Ctrl Pts',(15.509210476167,2.08166817117217E-16,
11.0246348408465));
#7177=CARTESIAN_POINT('Origin',(0.25,0.,0.));
#7178=CARTESIAN_POINT('',(0.5,-5.78383980645509E-16,-4.72286361298787));
#7179=CARTESIAN_POINT('',(0.5,-5.78383980645509E-16,4.72286361298787));
#7180=CARTESIAN_POINT('Origin',(0.5,0.,0.));
#7181=CARTESIAN_POINT('Origin',(0.5,0.,0.));
#7182=CARTESIAN_POINT('',(0.,5.17151640688142E-16,-4.22286361298787));
#7183=CARTESIAN_POINT('',(0.25,5.47767810666826E-16,-4.47286361298787));
#7184=CARTESIAN_POINT('Origin',(0.,0.,0.));
#7185=CARTESIAN_POINT('Origin',(0.,0.,-4.72286361298787));
#7186=CARTESIAN_POINT('',(0.,-4.55919300730774E-16,3.72286361298787));
#7187=CARTESIAN_POINT('Origin',(0.,0.,0.));
#7188=CARTESIAN_POINT('Origin',(5.01066115876088,0.,0.));
#7189=CARTESIAN_POINT('',(10.0213223175218,-5.78383980645509E-16,4.72286361298787));
#7190=CARTESIAN_POINT('Origin',(10.0213223175218,0.,0.));
#7191=CARTESIAN_POINT('',(5.01066115876088,-5.78383980645509E-16,4.72286361298787));
#7192=CARTESIAN_POINT('Origin',(29.5129125498419,0.,0.));
#7193=CARTESIAN_POINT('',(30.0129125498419,-1.28889603700374E-15,10.5246348408465));
#7194=CARTESIAN_POINT('Origin',(30.0129125498419,0.,0.));
#7195=CARTESIAN_POINT('',(29.5129125498419,-1.3501283769611E-15,11.0246348408465));
#7196=CARTESIAN_POINT('Origin',(29.5129125498419,-1.28889603700374E-15,
10.5246348408465));
#7197=CARTESIAN_POINT('Origin',(29.5129125498419,0.,0.));
#7198=CARTESIAN_POINT('Origin',(20.0171174336818,0.,0.));
#7199=CARTESIAN_POINT('',(20.0171174336818,-1.3501283769611E-15,11.0246348408465));
#7200=CARTESIAN_POINT('',(20.0171174336818,-1.3501283769611E-15,11.0246348408465));
#7201=CARTESIAN_POINT('',(10.5213223175218,-1.3501283769611E-15,11.0246348408465));
#7202=CARTESIAN_POINT('',(20.0171174336818,-1.3501283769611E-15,11.0246348408465));
#7203=CARTESIAN_POINT('Origin',(10.5213223175218,0.,0.));
#7204=CARTESIAN_POINT('Origin',(30.0129125498419,0.,-10.0246348408465));
#7205=CARTESIAN_POINT('Origin',(10.5213223175218,0.,0.));
#7206=CARTESIAN_POINT('',(10.0213223175218,-1.28889603700374E-15,10.5246348408465));
#7207=CARTESIAN_POINT('Origin',(10.5213223175218,-1.28889603700374E-15,
10.5246348408465));
#7208=CARTESIAN_POINT('Origin',(10.0213223175218,0.,0.));
#7209=CARTESIAN_POINT('Origin',(10.0213223175218,0.,-11.0246348408465));
#7210=CARTESIAN_POINT('Origin',(14.0224984115252,0.,-3.72286361298787));
#7211=CARTESIAN_POINT('',(14.0224984115252,-4.55919300730774E-16,3.72286361298787));
#7212=CARTESIAN_POINT('Origin',(14.0224984115252,0.,0.));
#7213=CARTESIAN_POINT('Origin',(7.01124920576262,0.,0.));
#7214=CARTESIAN_POINT('',(7.01124920576262,-4.55919300730774E-16,3.72286361298787));
#7215=CARTESIAN_POINT('',(0.,0.,0.));
#7216=CARTESIAN_POINT('Origin',(-9.1,0.,0.));
#7217=CARTESIAN_POINT('',(-9.3288415129767,-1.81546672613512E-16,1.48244108211373));
#7218=CARTESIAN_POINT('',(-9.3288415129767,-2.80250026378947E-17,-1.48244108211373));
#7219=CARTESIAN_POINT('Origin',(-9.3288415129767,0.,0.));
#7220=CARTESIAN_POINT('',(-9.1,-1.12481983699639E-32,1.5));
#7221=CARTESIAN_POINT('Origin',(-9.1,0.,0.));
#7222=CARTESIAN_POINT('Origin',(-9.3288415129767,0.,0.));
#7223=CARTESIAN_POINT('',(-9.1,-1.12481983699639E-32,-1.5));
#7224=CARTESIAN_POINT('Origin',(-9.1,0.,0.));
#7225=CARTESIAN_POINT('Origin',(-9.3288415129767,0.,2.17791759537647));
#7226=CARTESIAN_POINT('',(-9.3288415129767,-1.85786336178794E-16,1.51706056234455));
#7227=CARTESIAN_POINT('Origin',(-9.3288415129767,0.,0.));
#7228=CARTESIAN_POINT('Origin',(-6.41326808244201,0.,0.));
#7229=CARTESIAN_POINT('',(-6.41326808244201,-1.85786336178794E-16,1.51706056234455));
#7230=CARTESIAN_POINT('Origin',(-6.41326808244201,0.,0.));
#7231=CARTESIAN_POINT('Origin',(-8.11443509544501,0.,0.));
#7232=CARTESIAN_POINT('',(-8.11443509544501,-1.85786336178794E-16,1.51706056234455));
#7233=CARTESIAN_POINT('',(0.,0.,0.));
#7234=CARTESIAN_POINT('Origin',(-7.75,0.,0.));
#7235=CARTESIAN_POINT('',(-8.,3.22286361298787,3.94686960773406E-16));
#7236=CARTESIAN_POINT('Origin',(-8.,0.,0.));
#7237=CARTESIAN_POINT('',(-7.5,3.72286361298787,-4.55919300730774E-16));
#7238=CARTESIAN_POINT('',(-7.75,3.47286361298787,-4.2530313075209E-16));
#7239=CARTESIAN_POINT('Origin',(-7.5,0.,0.));
#7240=CARTESIAN_POINT('Origin',(-8.,0.,0.));
#7241=CARTESIAN_POINT('',(-8.,-1.85786336178794E-16,1.51706056234455));
#7242=CARTESIAN_POINT('Origin',(-8.,0.,0.));
#7243=CARTESIAN_POINT('Origin',(0.,0.,0.));
#7244=CARTESIAN_POINT('',(21.22,3.72286361298787,-4.55919300730774E-16));
#7245=CARTESIAN_POINT('Origin',(21.22,0.,0.));
#7246=CARTESIAN_POINT('',(0.,3.72286361298787,4.55919300730774E-16));
#7247=CARTESIAN_POINT('Origin',(-6.41326808244201,0.,0.));
#7248=CARTESIAN_POINT('',(-6.41326808244201,-1.85786336178794E-16,1.51706056234455));
#7249=CARTESIAN_POINT('Origin',(-6.41326808244201,0.,0.));
#7250=CARTESIAN_POINT('Origin',(-8.11443509544501,0.,0.));
#7251=CARTESIAN_POINT('',(-8.11443509544501,-1.85786336178794E-16,1.51706056234455));
#7252=CARTESIAN_POINT('Origin',(21.22,0.,0.));
#7253=CARTESIAN_POINT('',(0.,0.,0.));
#7254=CARTESIAN_POINT('Origin',(-9.1,0.,0.));
#7255=CARTESIAN_POINT('',(-9.1,-1.12481983699639E-32,1.5));
#7256=CARTESIAN_POINT('',(-9.1,-1.12481983699639E-32,-1.5));
#7257=CARTESIAN_POINT('Origin',(-9.1,0.,0.));
#7258=CARTESIAN_POINT('',(0.,0.,0.));
#7259=CARTESIAN_POINT('Origin',(52.9998593353039,0.,0.));
#7260=CARTESIAN_POINT('',(57.9998593353039,-2.,-2.44929359829471E-16));
#7261=CARTESIAN_POINT('Origin',(57.9998593353039,0.,0.));
#7262=CARTESIAN_POINT('',(52.9998593353039,-2.,-2.44929359829471E-16));
#7263=CARTESIAN_POINT('',(52.9998593353039,-2.,-2.44929359829471E-16));
#7264=CARTESIAN_POINT('Origin',(52.9998593353039,0.,0.));
#7265=CARTESIAN_POINT('Origin',(57.9998593353039,0.,0.));
#7266=CARTESIAN_POINT('Origin',(52.9998593353039,0.,0.));
#7267=CARTESIAN_POINT('',(0.,0.,0.));
#7268=CARTESIAN_POINT('Origin',(21.2197085942866,0.,0.));
#7269=CARTESIAN_POINT('',(20.2197085942866,3.72286361298787,-4.55919300730774E-16));
#7270=CARTESIAN_POINT('Origin',(20.2197085942866,0.,0.));
#7271=CARTESIAN_POINT('',(21.2197085942866,3.72286361298787,-4.55919300730774E-16));
#7272=CARTESIAN_POINT('',(21.2197085942866,3.72286361298787,-4.55919300730774E-16));
#7273=CARTESIAN_POINT('Origin',(21.2197085942866,0.,0.));
#7274=CARTESIAN_POINT('Origin',(21.2197085942866,0.,0.));
#7275=CARTESIAN_POINT('',(20.2197085942866,5.22286361298787,-6.39616320602877E-16));
#7276=CARTESIAN_POINT('Origin',(20.2197085942866,0.,0.));
#7277=CARTESIAN_POINT('',(21.2197085942866,5.22286361298787,-6.39616320602877E-16));
#7278=CARTESIAN_POINT('',(21.2197085942866,5.22286361298787,-6.39616320602877E-16));
#7279=CARTESIAN_POINT('Origin',(21.2197085942866,0.,0.));
#7280=CARTESIAN_POINT('Origin',(20.2197085942866,0.,0.));
#7281=CARTESIAN_POINT('Origin',(21.2197085942866,0.,0.));
#7282=CARTESIAN_POINT('',(0.,0.,0.));
#7283=CARTESIAN_POINT('',(0.,0.,0.));
#7284=CARTESIAN_POINT('',(0.,0.,0.));
#7285=CARTESIAN_POINT('',(0.,0.,0.));
#7286=CARTESIAN_POINT('',(0.,0.,0.));
#7287=CARTESIAN_POINT('',(0.,0.,0.));
#7288=CARTESIAN_POINT('',(0.,0.,0.));
#7289=CARTESIAN_POINT('',(0.,0.,0.));
#7290=CARTESIAN_POINT('',(0.,0.,0.));
#7291=CARTESIAN_POINT('',(0.,0.,0.));
#7292=UNCERTAINTY_MEASURE_WITH_UNIT(LENGTH_MEASURE(0.01),#7316,
'DISTANCE_ACCURACY_VALUE',
'Maximum model space distance between geometric entities at asserted c
onnectivities');
#7293=UNCERTAINTY_MEASURE_WITH_UNIT(LENGTH_MEASURE(0.01),#7316,
'DISTANCE_ACCURACY_VALUE',
'Maximum model space distance between geometric entities at asserted c
onnectivities');
#7294=UNCERTAINTY_MEASURE_WITH_UNIT(LENGTH_MEASURE(0.01),#7316,
'DISTANCE_ACCURACY_VALUE',
'Maximum model space distance between geometric entities at asserted c
onnectivities');
#7295=UNCERTAINTY_MEASURE_WITH_UNIT(LENGTH_MEASURE(0.01),#7316,
'DISTANCE_ACCURACY_VALUE',
'Maximum model space distance between geometric entities at asserted c
onnectivities');
#7296=UNCERTAINTY_MEASURE_WITH_UNIT(LENGTH_MEASURE(0.01),#7316,
'DISTANCE_ACCURACY_VALUE',
'Maximum model space distance between geometric entities at asserted c
onnectivities');
#7297=UNCERTAINTY_MEASURE_WITH_UNIT(LENGTH_MEASURE(0.01),#7316,
'DISTANCE_ACCURACY_VALUE',
'Maximum model space distance between geometric entities at asserted c
onnectivities');
#7298=UNCERTAINTY_MEASURE_WITH_UNIT(LENGTH_MEASURE(0.01),#7316,
'DISTANCE_ACCURACY_VALUE',
'Maximum model space distance between geometric entities at asserted c
onnectivities');
#7299=UNCERTAINTY_MEASURE_WITH_UNIT(LENGTH_MEASURE(0.01),#7316,
'DISTANCE_ACCURACY_VALUE',
'Maximum model space distance between geometric entities at asserted c
onnectivities');
#7300=UNCERTAINTY_MEASURE_WITH_UNIT(LENGTH_MEASURE(0.01),#7316,
'DISTANCE_ACCURACY_VALUE',
'Maximum model space distance between geometric entities at asserted c
onnectivities');
#7301=UNCERTAINTY_MEASURE_WITH_UNIT(LENGTH_MEASURE(0.01),#7316,
'DISTANCE_ACCURACY_VALUE',
'Maximum model space distance between geometric entities at asserted c
onnectivities');
#7302=UNCERTAINTY_MEASURE_WITH_UNIT(LENGTH_MEASURE(0.01),#7316,
'DISTANCE_ACCURACY_VALUE',
'Maximum model space distance between geometric entities at asserted c
onnectivities');
#7303=UNCERTAINTY_MEASURE_WITH_UNIT(LENGTH_MEASURE(0.01),#7316,
'DISTANCE_ACCURACY_VALUE',
'Maximum model space distance between geometric entities at asserted c
onnectivities');
#7304=(
GEOMETRIC_REPRESENTATION_CONTEXT(3)
GLOBAL_UNCERTAINTY_ASSIGNED_CONTEXT((#7292))
GLOBAL_UNIT_ASSIGNED_CONTEXT((#7316,#7318,#7319))
REPRESENTATION_CONTEXT('','3D')
);
#7305=(
GEOMETRIC_REPRESENTATION_CONTEXT(3)
GLOBAL_UNCERTAINTY_ASSIGNED_CONTEXT((#7293))
GLOBAL_UNIT_ASSIGNED_CONTEXT((#7316,#7318,#7319))
REPRESENTATION_CONTEXT('','3D')
);
#7306=(
GEOMETRIC_REPRESENTATION_CONTEXT(3)
GLOBAL_UNCERTAINTY_ASSIGNED_CONTEXT((#7294))
GLOBAL_UNIT_ASSIGNED_CONTEXT((#7316,#7318,#7319))
REPRESENTATION_CONTEXT('','3D')
);
#7307=(
GEOMETRIC_REPRESENTATION_CONTEXT(3)
GLOBAL_UNCERTAINTY_ASSIGNED_CONTEXT((#7295))
GLOBAL_UNIT_ASSIGNED_CONTEXT((#7316,#7318,#7319))
REPRESENTATION_CONTEXT('','3D')
);
#7308=(
GEOMETRIC_REPRESENTATION_CONTEXT(3)
GLOBAL_UNCERTAINTY_ASSIGNED_CONTEXT((#7296))
GLOBAL_UNIT_ASSIGNED_CONTEXT((#7316,#7318,#7319))
REPRESENTATION_CONTEXT('','3D')
);
#7309=(
GEOMETRIC_REPRESENTATION_CONTEXT(3)
GLOBAL_UNCERTAINTY_ASSIGNED_CONTEXT((#7297))
GLOBAL_UNIT_ASSIGNED_CONTEXT((#7316,#7318,#7319))
REPRESENTATION_CONTEXT('','3D')
);
#7310=(
GEOMETRIC_REPRESENTATION_CONTEXT(3)
GLOBAL_UNCERTAINTY_ASSIGNED_CONTEXT((#7298))
GLOBAL_UNIT_ASSIGNED_CONTEXT((#7316,#7318,#7319))
REPRESENTATION_CONTEXT('','3D')
);
#7311=(
GEOMETRIC_REPRESENTATION_CONTEXT(3)
GLOBAL_UNCERTAINTY_ASSIGNED_CONTEXT((#7299))
GLOBAL_UNIT_ASSIGNED_CONTEXT((#7316,#7318,#7319))
REPRESENTATION_CONTEXT('','3D')
);
#7312=(
GEOMETRIC_REPRESENTATION_CONTEXT(3)
GLOBAL_UNCERTAINTY_ASSIGNED_CONTEXT((#7300))
GLOBAL_UNIT_ASSIGNED_CONTEXT((#7316,#7318,#7319))
REPRESENTATION_CONTEXT('','3D')
);
#7313=(
GEOMETRIC_REPRESENTATION_CONTEXT(3)
GLOBAL_UNCERTAINTY_ASSIGNED_CONTEXT((#7301))
GLOBAL_UNIT_ASSIGNED_CONTEXT((#7316,#7318,#7319))
REPRESENTATION_CONTEXT('','3D')
);
#7314=(
GEOMETRIC_REPRESENTATION_CONTEXT(3)
GLOBAL_UNCERTAINTY_ASSIGNED_CONTEXT((#7302))
GLOBAL_UNIT_ASSIGNED_CONTEXT((#7316,#7318,#7319))
REPRESENTATION_CONTEXT('','3D')
);
#7315=(
GEOMETRIC_REPRESENTATION_CONTEXT(3)
GLOBAL_UNCERTAINTY_ASSIGNED_CONTEXT((#7303))
GLOBAL_UNIT_ASSIGNED_CONTEXT((#7316,#7318,#7319))
REPRESENTATION_CONTEXT('','3D')
);
#7316=(
LENGTH_UNIT()
NAMED_UNIT(*)
SI_UNIT(.MILLI.,.METRE.)
);
#7317=(
LENGTH_UNIT()
NAMED_UNIT(*)
SI_UNIT($,.METRE.)
);
#7318=(
NAMED_UNIT(*)
PLANE_ANGLE_UNIT()
SI_UNIT($,.RADIAN.)
);
#7319=(
NAMED_UNIT(*)
SI_UNIT($,.STERADIAN.)
SOLID_ANGLE_UNIT()
);
#7320=SHAPE_DEFINITION_REPRESENTATION(#7331,#7352);
#7321=SHAPE_DEFINITION_REPRESENTATION(#7332,#7353);
#7322=SHAPE_DEFINITION_REPRESENTATION(#7333,#7354);
#7323=SHAPE_DEFINITION_REPRESENTATION(#7334,#7355);
#7324=SHAPE_DEFINITION_REPRESENTATION(#7335,#7356);
#7325=SHAPE_DEFINITION_REPRESENTATION(#7336,#7357);
#7326=SHAPE_DEFINITION_REPRESENTATION(#7337,#7358);
#7327=SHAPE_DEFINITION_REPRESENTATION(#7338,#7359);
#7328=SHAPE_DEFINITION_REPRESENTATION(#7339,#7360);
#7329=SHAPE_DEFINITION_REPRESENTATION(#7340,#7361);
#7330=SHAPE_DEFINITION_REPRESENTATION(#7341,#7362);
#7331=PRODUCT_DEFINITION_SHAPE('',$,#7364);
#7332=PRODUCT_DEFINITION_SHAPE('',$,#7365);
#7333=PRODUCT_DEFINITION_SHAPE('',$,#7366);
#7334=PRODUCT_DEFINITION_SHAPE('',$,#7367);
#7335=PRODUCT_DEFINITION_SHAPE('',$,#7368);
#7336=PRODUCT_DEFINITION_SHAPE('',$,#7369);
#7337=PRODUCT_DEFINITION_SHAPE('',$,#7370);
#7338=PRODUCT_DEFINITION_SHAPE('',$,#7371);
#7339=PRODUCT_DEFINITION_SHAPE('',$,#7372);
#7340=PRODUCT_DEFINITION_SHAPE('',$,#7373);
#7341=PRODUCT_DEFINITION_SHAPE('',$,#7374);
#7342=PRODUCT_DEFINITION_SHAPE($,$,#41);
#7343=PRODUCT_DEFINITION_SHAPE($,$,#42);
#7344=PRODUCT_DEFINITION_SHAPE($,$,#43);
#7345=PRODUCT_DEFINITION_SHAPE($,$,#44);
#7346=PRODUCT_DEFINITION_SHAPE($,$,#45);
#7347=PRODUCT_DEFINITION_SHAPE($,$,#46);
#7348=PRODUCT_DEFINITION_SHAPE($,$,#47);
#7349=PRODUCT_DEFINITION_SHAPE($,$,#48);
#7350=PRODUCT_DEFINITION_SHAPE($,$,#49);
#7351=PRODUCT_DEFINITION_SHAPE($,$,#50);
#7352=SHAPE_REPRESENTATION('',(#3335,#3714,#3715,#3716,#3717,#3718,#3719,
#3720,#3721,#3722,#3723),#7304);
#7353=SHAPE_REPRESENTATION('',(#3336),#7305);
#7354=SHAPE_REPRESENTATION('',(#3452),#7306);
#7355=SHAPE_REPRESENTATION('',(#3467),#7307);
#7356=SHAPE_REPRESENTATION('',(#3527),#7308);
#7357=SHAPE_REPRESENTATION('',(#3638),#7309);
#7358=SHAPE_REPRESENTATION('',(#3673),#7310);
#7359=SHAPE_REPRESENTATION('',(#3684),#7311);
#7360=SHAPE_REPRESENTATION('',(#3696),#7312);
#7361=SHAPE_REPRESENTATION('',(#3699),#7313);
#7362=SHAPE_REPRESENTATION('',(#3705),#7314);
#7363=PRODUCT_DEFINITION_CONTEXT('part definition',#7398,'design');
#7364=PRODUCT_DEFINITION('MAS-283','MAS-283',#7375,#7363);
#7365=PRODUCT_DEFINITION('End_Cap','End_Cap',#7376,#7363);
#7366=PRODUCT_DEFINITION('Locking_Ring','Locking_Ring',#7377,#7363);
#7367=PRODUCT_DEFINITION('Knob','Knob',#7378,#7363);
#7368=PRODUCT_DEFINITION('Middle_Ring','Middle_Ring',#7379,#7363);
#7369=PRODUCT_DEFINITION('Main_Housing','Main_Housing',#7380,#7363);
#7370=PRODUCT_DEFINITION('Plunger_Pin','Plunger_Pin',#7381,#7363);
#7371=PRODUCT_DEFINITION('Plunger_Shaft','Plunger_Shaft',#7382,#7363);
#7372=PRODUCT_DEFINITION('Ball','Ball',#7383,#7363);
#7373=PRODUCT_DEFINITION('Shaft','Shaft',#7384,#7363);
#7374=PRODUCT_DEFINITION('Ring','Ring',#7385,#7363);
#7375=PRODUCT_DEFINITION_FORMATION('',$,#7400);
#7376=PRODUCT_DEFINITION_FORMATION('',$,#7401);
#7377=PRODUCT_DEFINITION_FORMATION('',$,#7402);
#7378=PRODUCT_DEFINITION_FORMATION('',$,#7403);
#7379=PRODUCT_DEFINITION_FORMATION('',$,#7404);
#7380=PRODUCT_DEFINITION_FORMATION('',$,#7405);
#7381=PRODUCT_DEFINITION_FORMATION('',$,#7406);
#7382=PRODUCT_DEFINITION_FORMATION('',$,#7407);
#7383=PRODUCT_DEFINITION_FORMATION('',$,#7408);
#7384=PRODUCT_DEFINITION_FORMATION('',$,#7409);
#7385=PRODUCT_DEFINITION_FORMATION('',$,#7410);
#7386=PRODUCT_RELATED_PRODUCT_CATEGORY('MAS-283','MAS-283',(#7400));
#7387=PRODUCT_RELATED_PRODUCT_CATEGORY('End_Cap','End_Cap',(#7401));
#7388=PRODUCT_RELATED_PRODUCT_CATEGORY('Locking_Ring','Locking_Ring',(#7402));
#7389=PRODUCT_RELATED_PRODUCT_CATEGORY('Knob','Knob',(#7403));
#7390=PRODUCT_RELATED_PRODUCT_CATEGORY('Middle_Ring','Middle_Ring',(#7404));
#7391=PRODUCT_RELATED_PRODUCT_CATEGORY('Main_Housing','Main_Housing',(#7405));
#7392=PRODUCT_RELATED_PRODUCT_CATEGORY('Plunger_Pin','Plunger_Pin',(#7406));
#7393=PRODUCT_RELATED_PRODUCT_CATEGORY('Plunger_Shaft','Plunger_Shaft',
(#7407));
#7394=PRODUCT_RELATED_PRODUCT_CATEGORY('Ball','Ball',(#7408));
#7395=PRODUCT_RELATED_PRODUCT_CATEGORY('Shaft','Shaft',(#7409));
#7396=PRODUCT_RELATED_PRODUCT_CATEGORY('Ring','Ring',(#7410));
#7397=APPLICATION_PROTOCOL_DEFINITION('international standard',
'automotive_design',2009,#7398);
#7398=APPLICATION_CONTEXT(
'Core Data for Automotive Mechanical Design Process');
#7399=PRODUCT_CONTEXT('part definition',#7398,'mechanical');
#7400=PRODUCT('MAS-283','MAS-283',$,(#7399));
#7401=PRODUCT('End_Cap','End_Cap',$,(#7399));
#7402=PRODUCT('Locking_Ring','Locking_Ring',$,(#7399));
#7403=PRODUCT('Knob','Knob',$,(#7399));
#7404=PRODUCT('Middle_Ring','Middle_Ring',$,(#7399));
#7405=PRODUCT('Main_Housing','Main_Housing',$,(#7399));
#7406=PRODUCT('Plunger_Pin','Plunger_Pin',$,(#7399));
#7407=PRODUCT('Plunger_Shaft','Plunger_Shaft',$,(#7399));
#7408=PRODUCT('Ball','Ball',$,(#7399));
#7409=PRODUCT('Shaft','Shaft',$,(#7399));
#7410=PRODUCT('Ring','Ring',$,(#7399));
#7411=PRESENTATION_STYLE_ASSIGNMENT((#7412));
#7412=SURFACE_STYLE_USAGE(.BOTH.,#7413);
#7413=SURFACE_SIDE_STYLE('',(#7414));
#7414=SURFACE_STYLE_FILL_AREA(#7415);
#7415=FILL_AREA_STYLE('Steel - Satin',(#7416));
#7416=FILL_AREA_STYLE_COLOUR('Steel - Satin',#7417);
#7417=COLOUR_RGB('Steel - Satin',0.627450980392157,0.627450980392157,0.627450980392157);
#7418=COLOUR_RGB('Dark Blue',0.08,0.2,0.34);
#7419=FILL_AREA_STYLE_COLOUR('',#7418);
#7420=FILL_AREA_STYLE('',(#7419));
#7421=SURFACE_STYLE_FILL_AREA(#7420);
#7422=SURFACE_SIDE_STYLE('',(#7421));
#7423=SURFACE_STYLE_USAGE(.BOTH.,#7422);
#7424=PRESENTATION_STYLE_ASSIGNMENT((#7423));
#7425=COLOUR_RGB('Light Blue',0.38,0.62,0.78);
#7426=FILL_AREA_STYLE_COLOUR('',#7425);
#7427=FILL_AREA_STYLE('',(#7426));
#7428=SURFACE_STYLE_FILL_AREA(#7427);
#7429=SURFACE_SIDE_STYLE('',(#7428));
#7430=SURFACE_STYLE_USAGE(.BOTH.,#7429);
#7431=PRESENTATION_STYLE_ASSIGNMENT((#7430));
#7432=COLOUR_RGB('Sky Blue',0.24,0.69,0.87);
#7433=FILL_AREA_STYLE_COLOUR('',#7432);
#7434=FILL_AREA_STYLE('',(#7433));
#7435=SURFACE_STYLE_FILL_AREA(#7434);
#7436=SURFACE_SIDE_STYLE('',(#7435));
#7437=SURFACE_STYLE_USAGE(.BOTH.,#7436);
#7438=PRESENTATION_STYLE_ASSIGNMENT((#7437));
#7439=COLOUR_RGB('Grey',0.48,0.52,0.57);
#7440=FILL_AREA_STYLE_COLOUR('',#7439);
#7441=FILL_AREA_STYLE('',(#7440));
#7442=SURFACE_STYLE_FILL_AREA(#7441);
#7443=SURFACE_SIDE_STYLE('',(#7442));
#7444=SURFACE_STYLE_USAGE(.BOTH.,#7443);
#7445=PRESENTATION_STYLE_ASSIGNMENT((#7444));
#7446=COLOUR_RGB('Black',0.12,0.14,0.17);
#7447=FILL_AREA_STYLE_COLOUR('',#7446);
#7448=FILL_AREA_STYLE('',(#7447));
#7449=SURFACE_STYLE_FILL_AREA(#7448);
#7450=SURFACE_SIDE_STYLE('',(#7449));
#7451=SURFACE_STYLE_USAGE(.BOTH.,#7450);
#7452=PRESENTATION_STYLE_ASSIGNMENT((#7451));
#7453=COLOUR_RGB('Off White',0.89,0.88,0.83);
#7454=FILL_AREA_STYLE_COLOUR('',#7453);
#7455=FILL_AREA_STYLE('',(#7454));
#7456=SURFACE_STYLE_FILL_AREA(#7455);
#7457=SURFACE_SIDE_STYLE('',(#7456));
#7458=SURFACE_STYLE_USAGE(.BOTH.,#7457);
#7459=PRESENTATION_STYLE_ASSIGNMENT((#7458));
ENDSEC;
END-ISO-10303-21;
